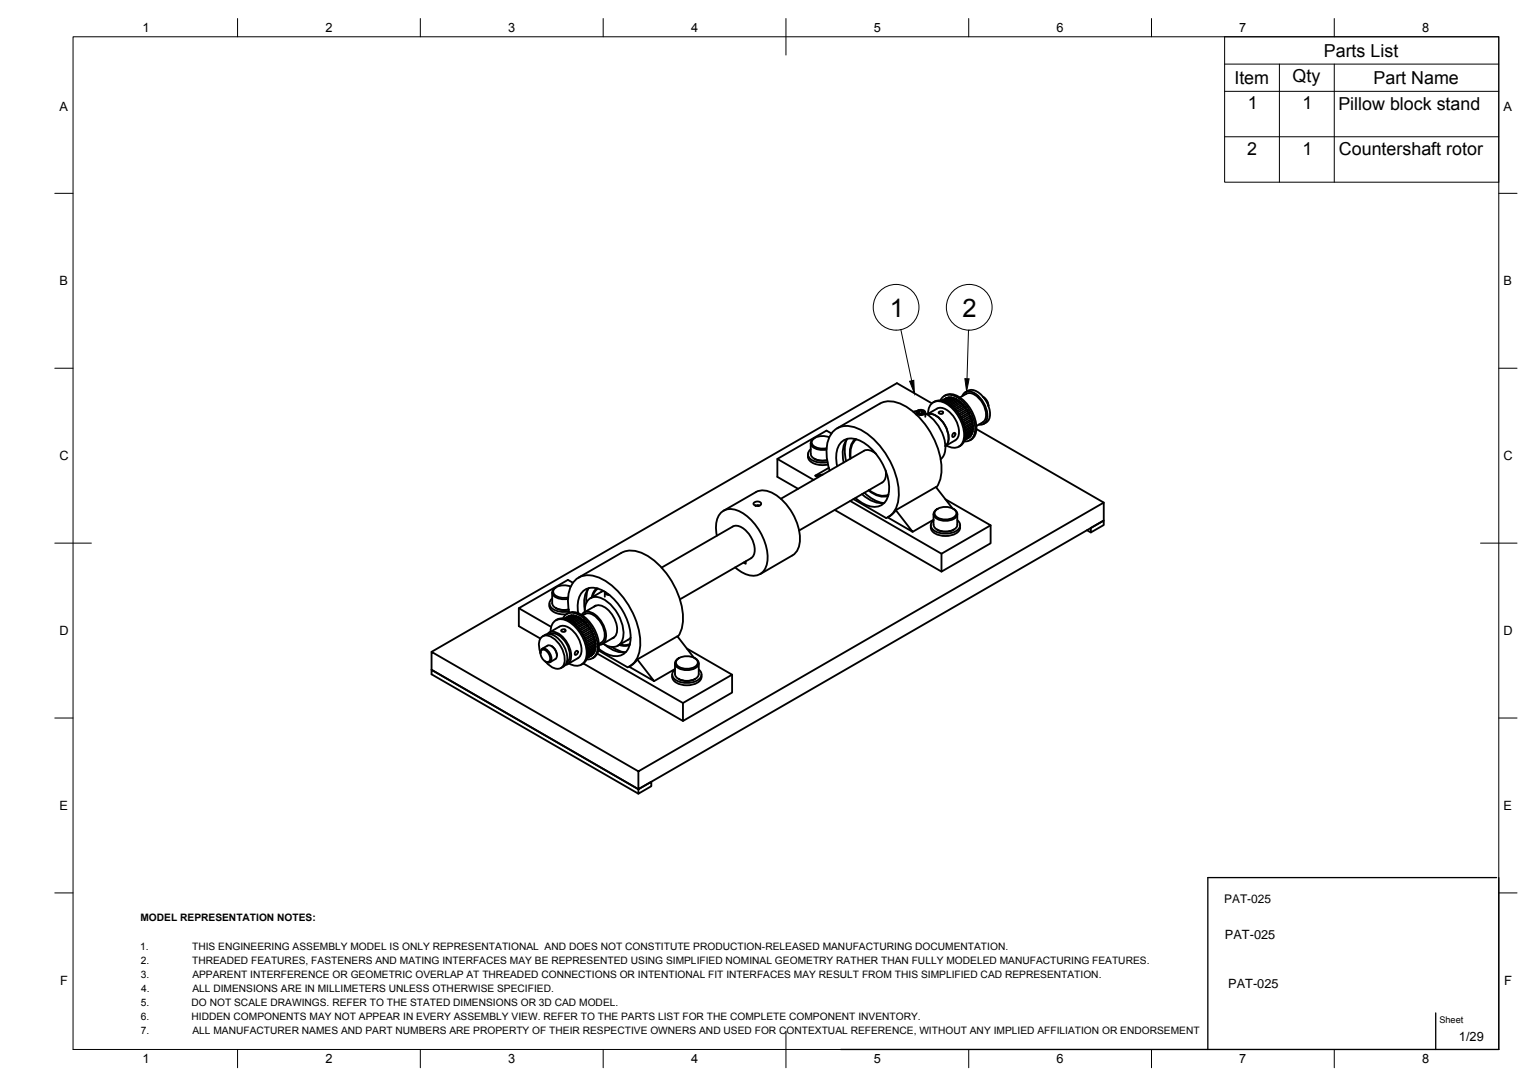
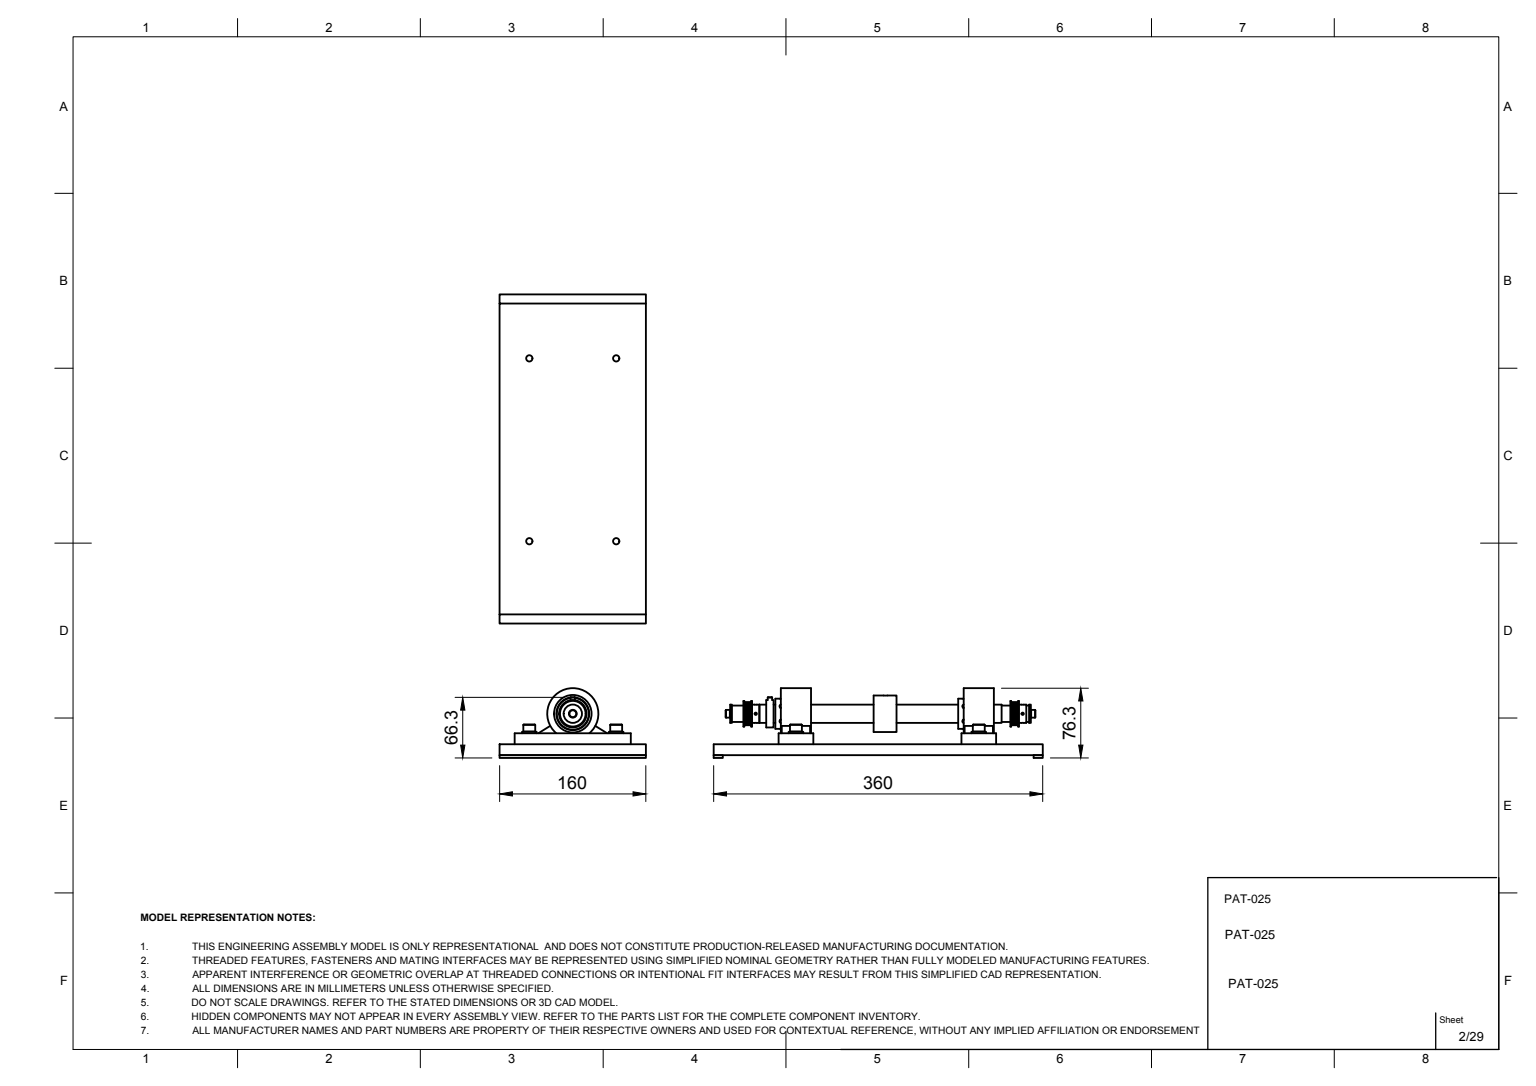
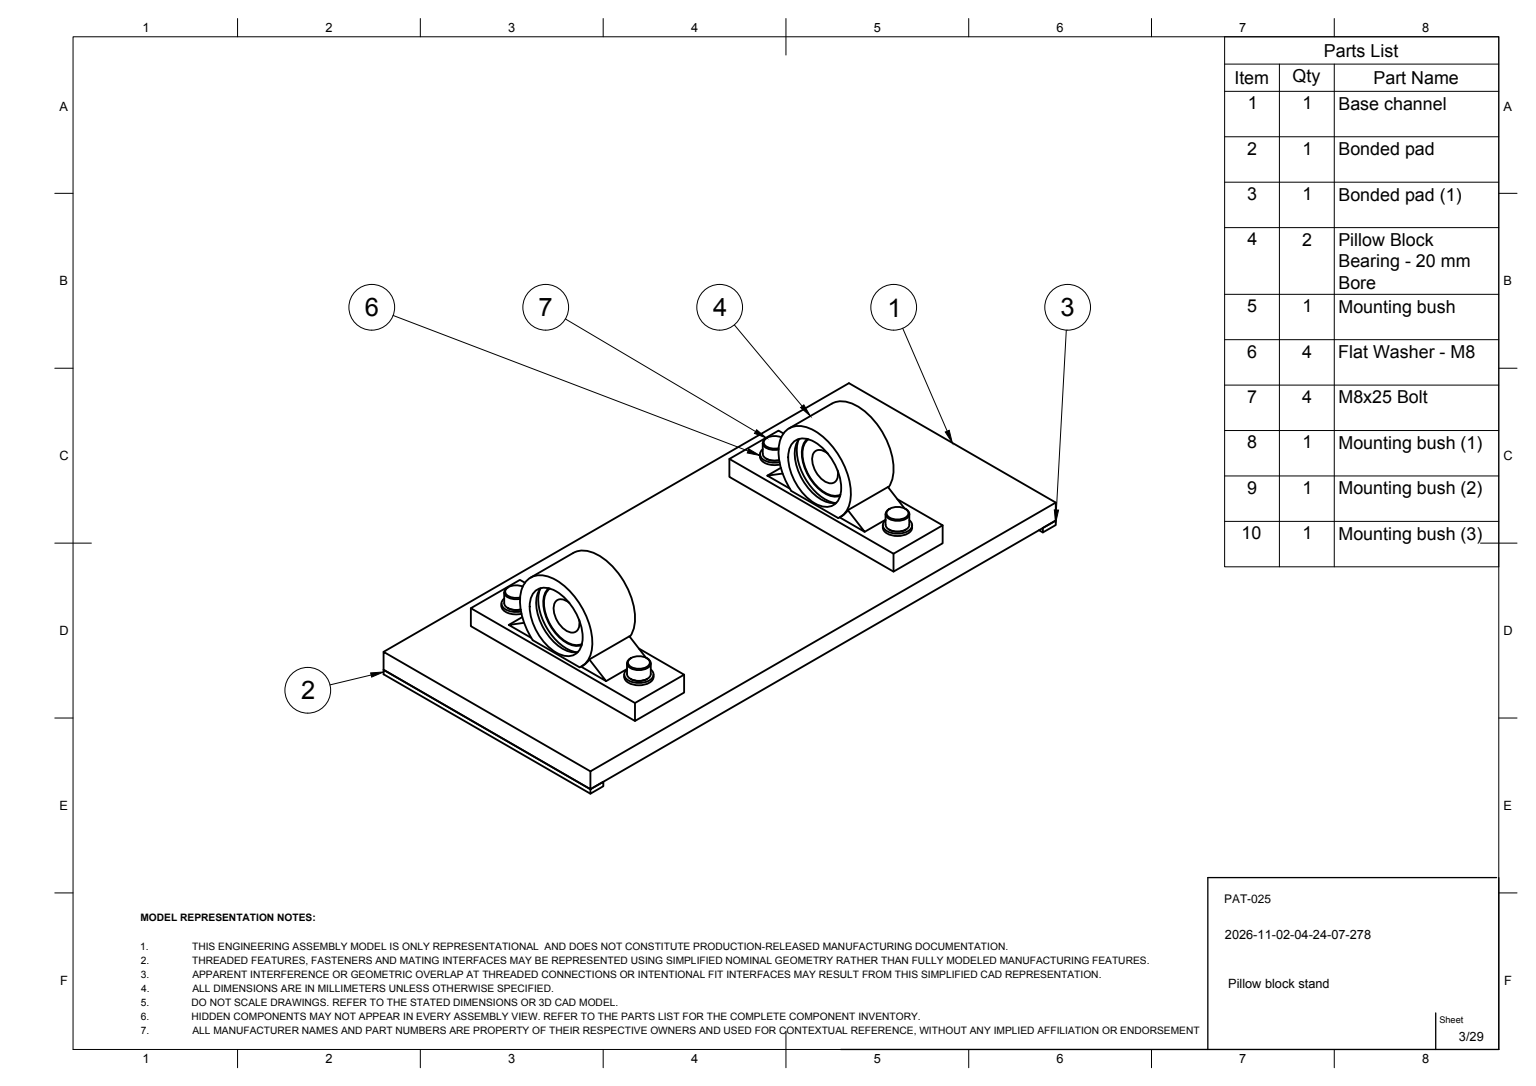
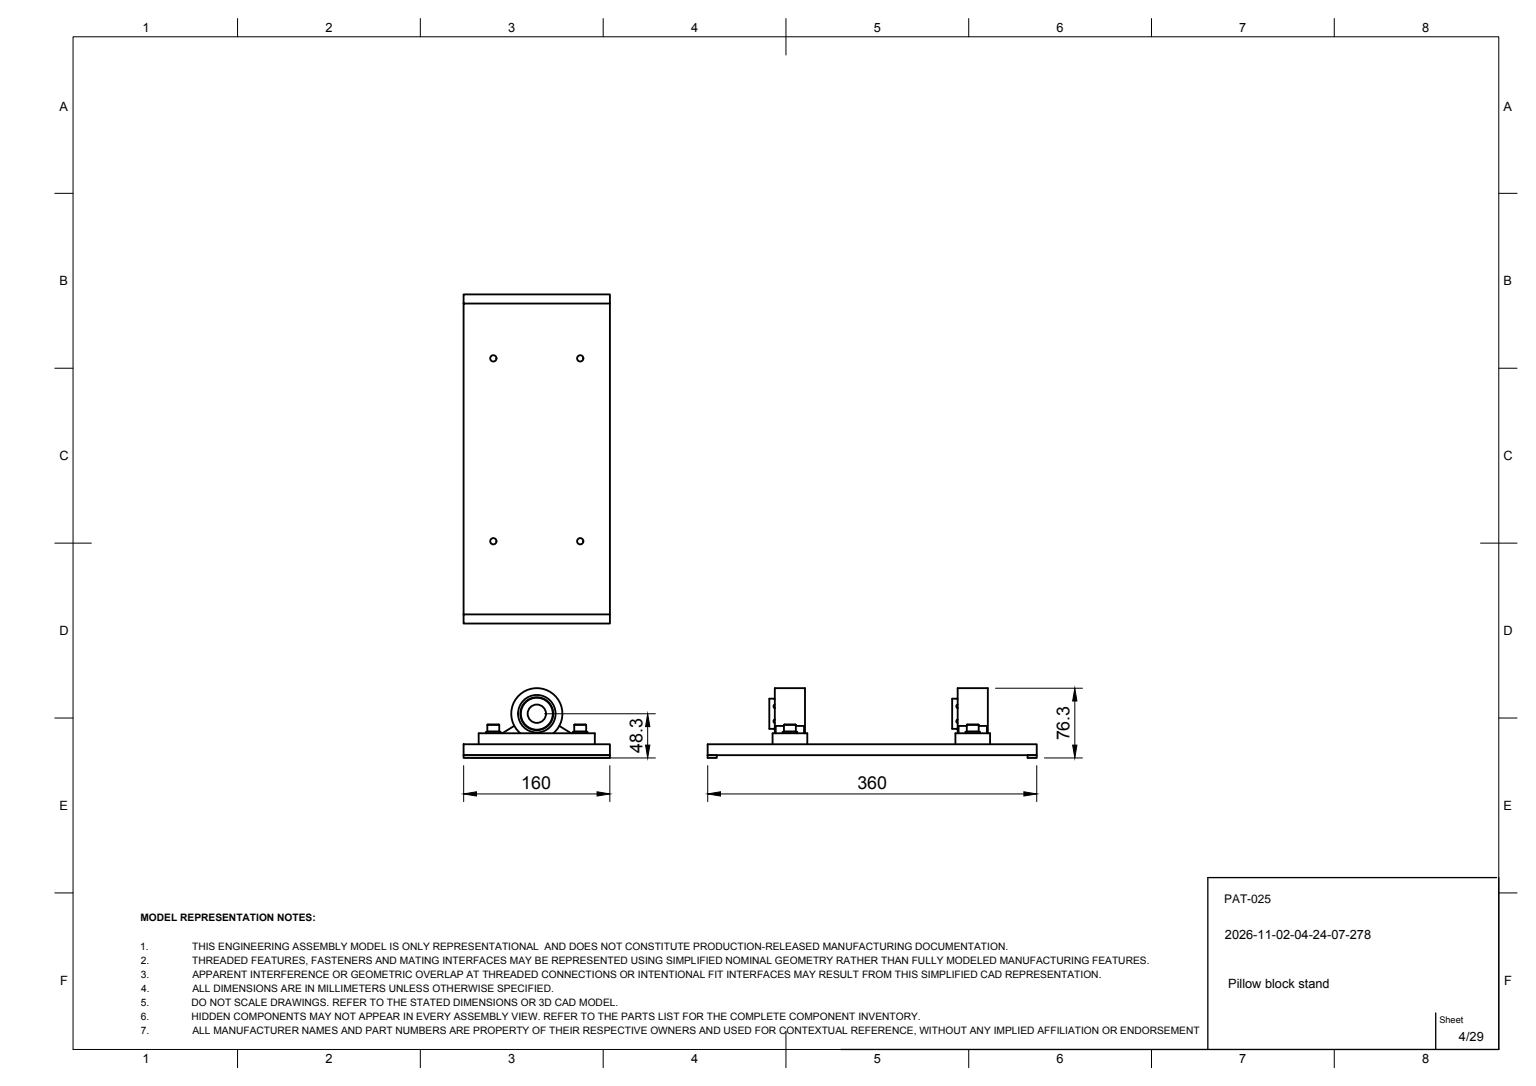
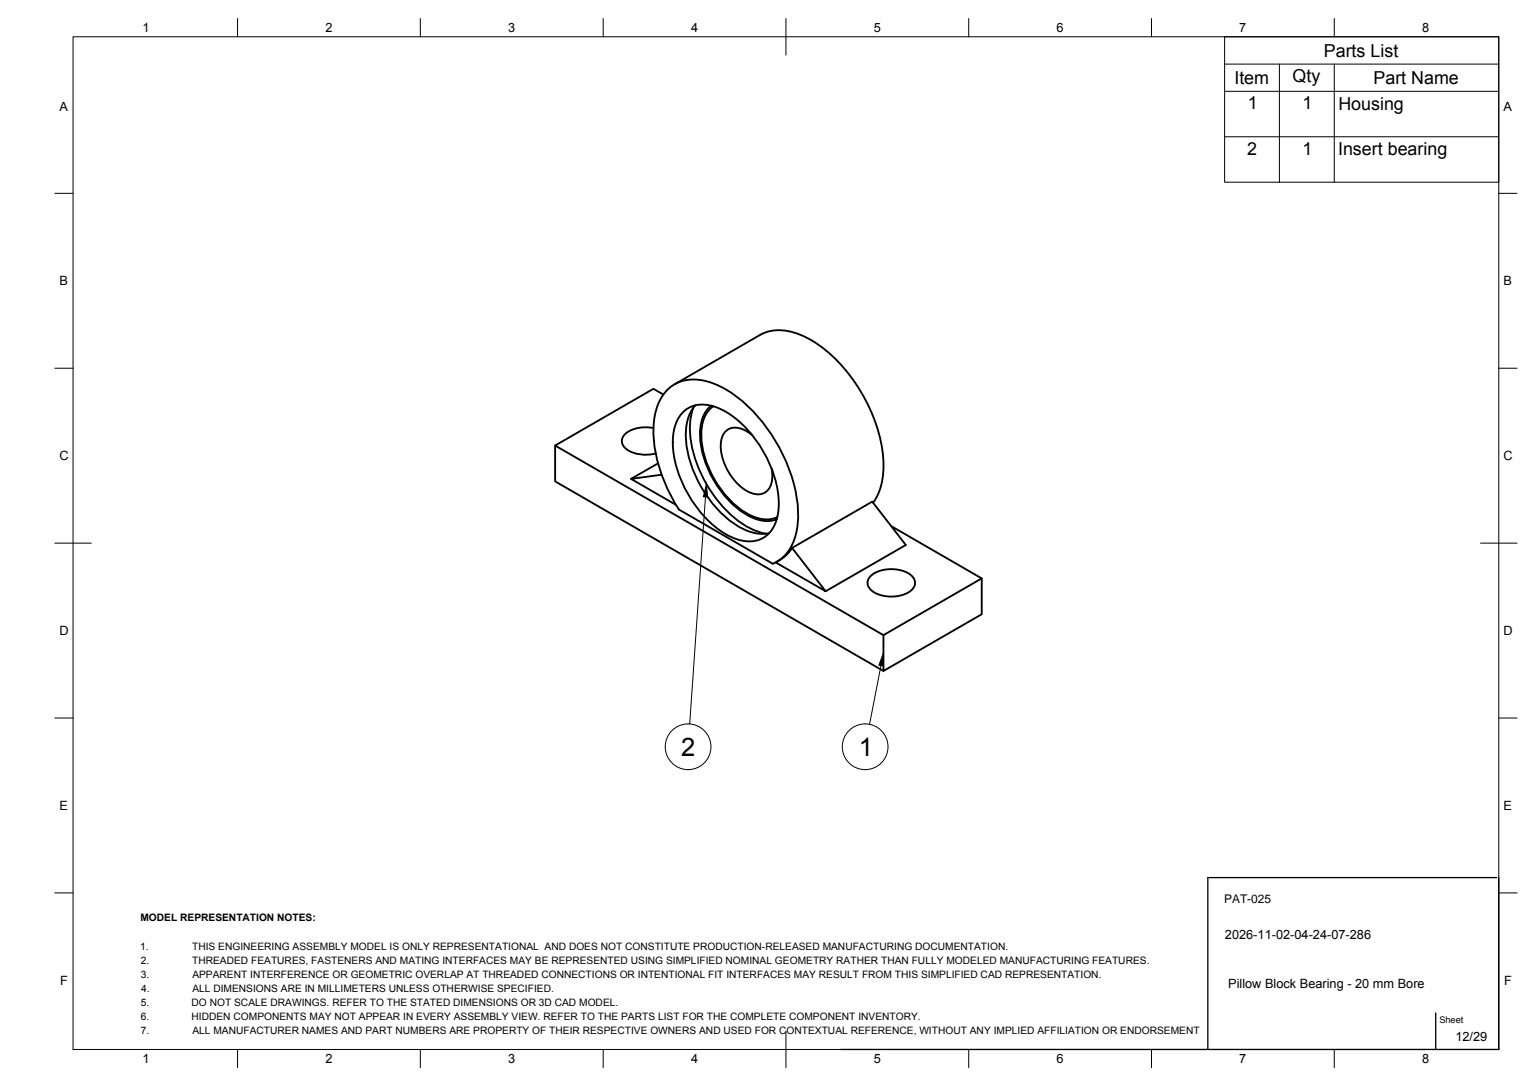
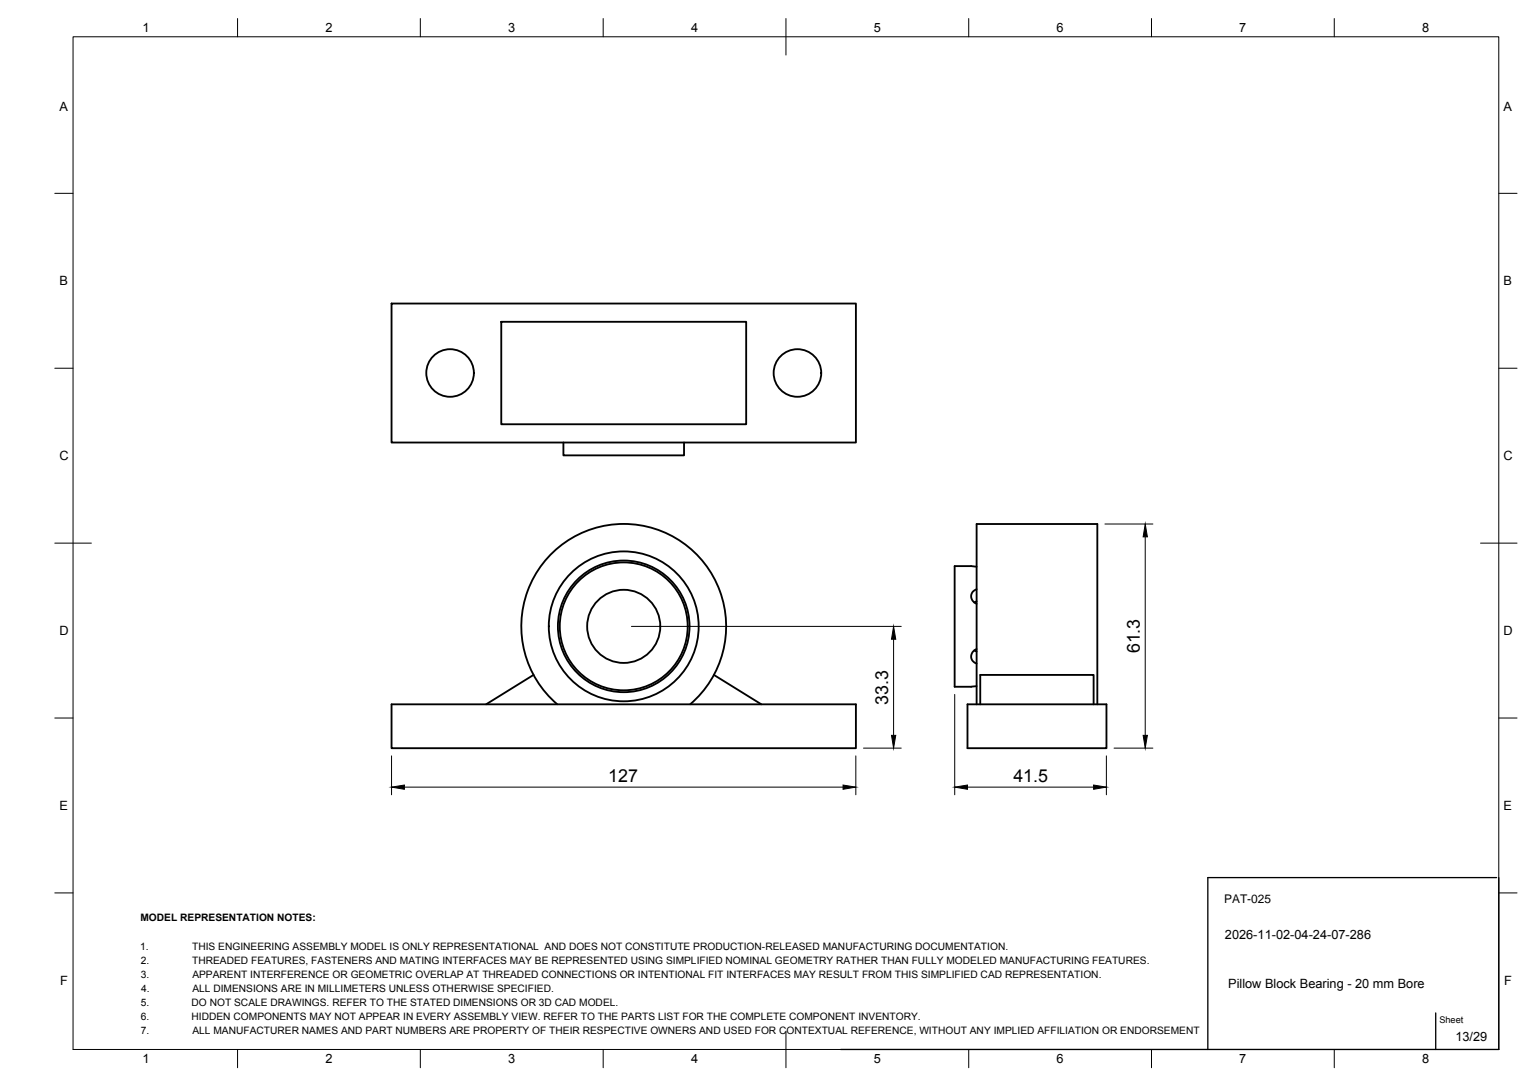
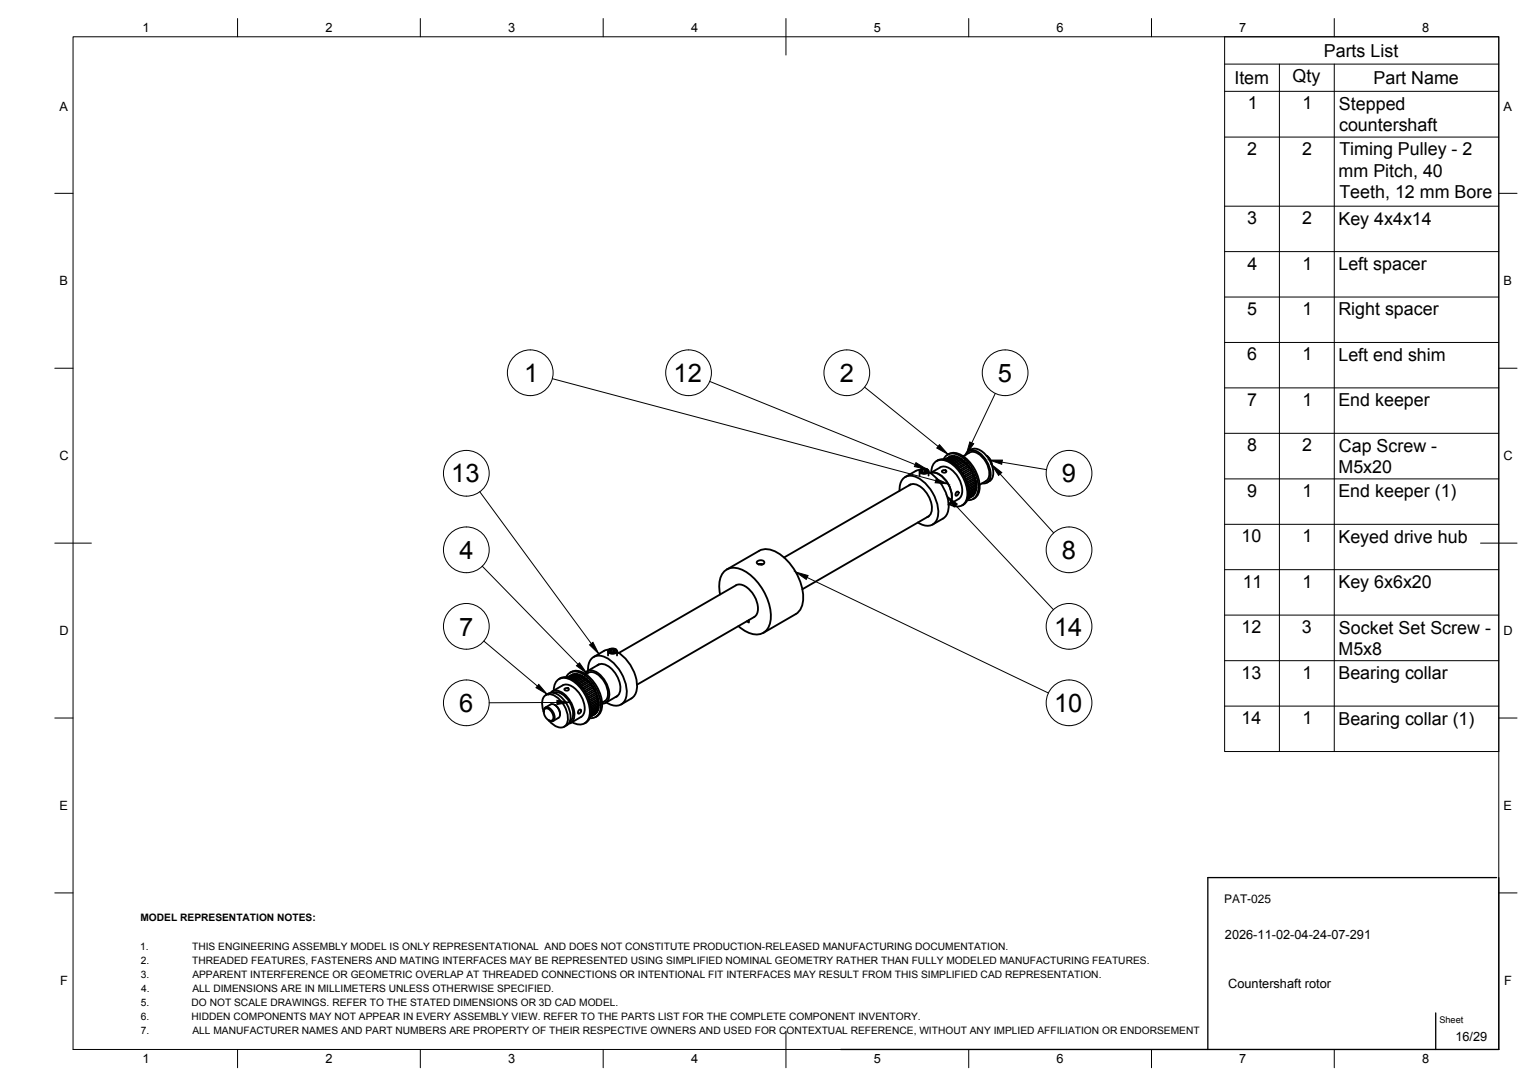
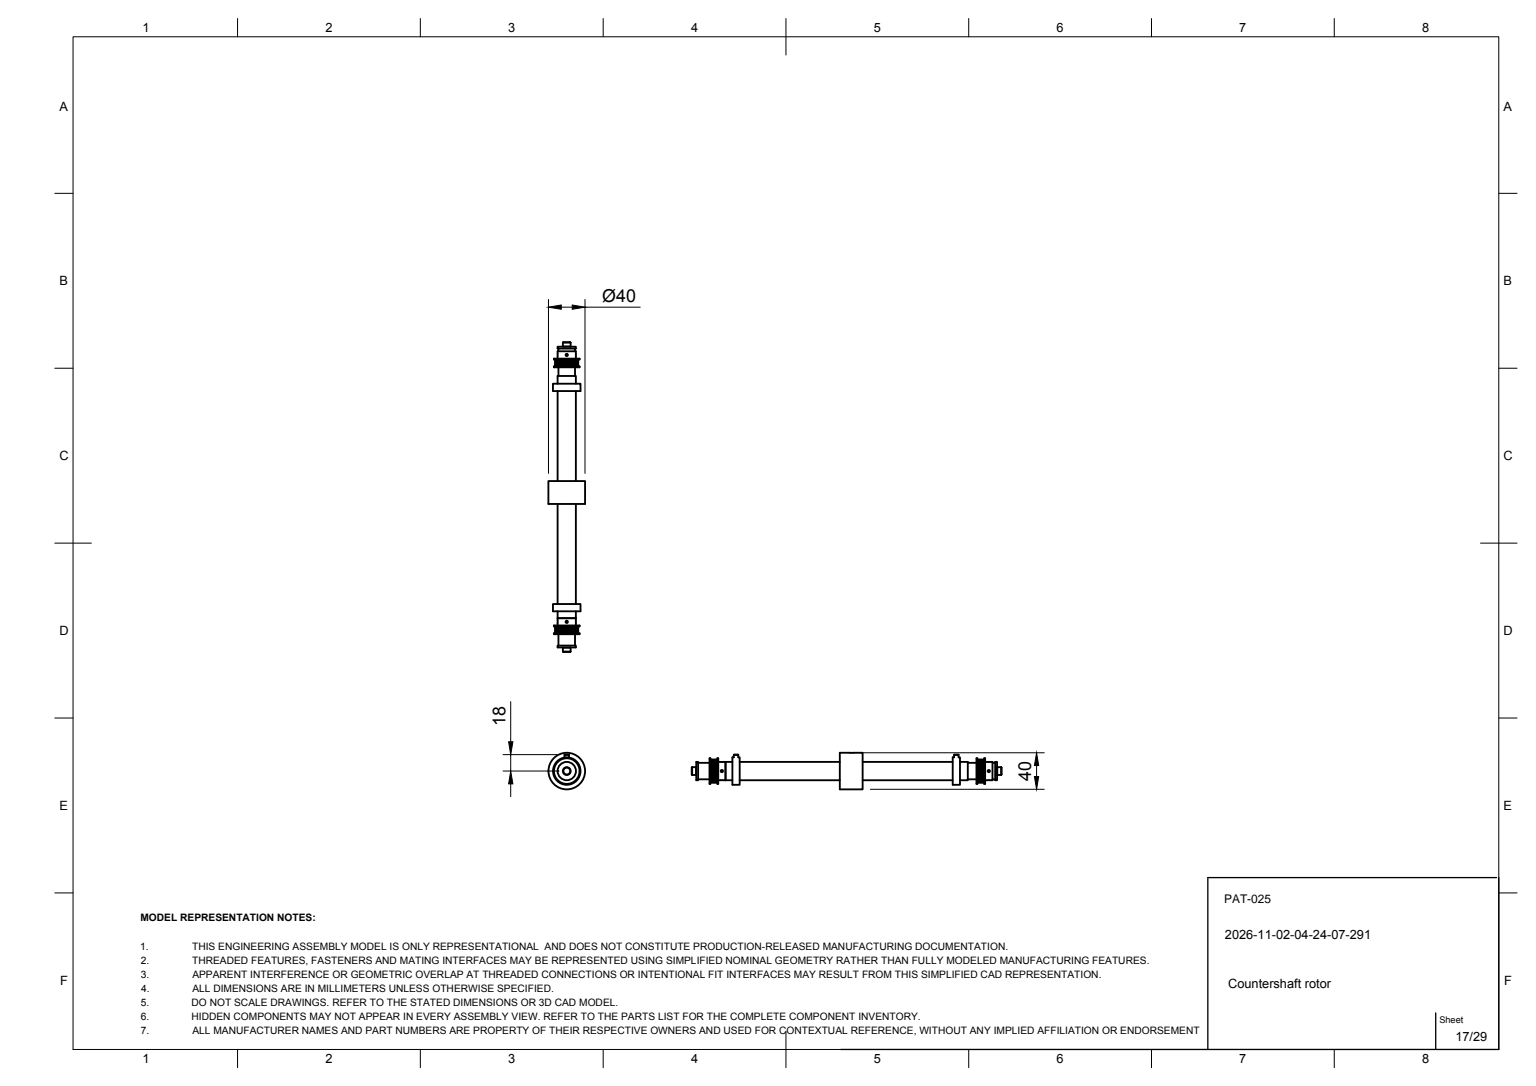
ISO-10303-21;
HEADER;
/* Generated by software containing ST-Developer
 * from STEP Tools, Inc. (www.steptools.com) 
 */

FILE_DESCRIPTION(
/* description */ ('Counter shaft with two pulleys and keyed hub'),
/* implementation_level */ '2;1');

FILE_NAME(
/* name */ 'PAT-025',
/* time_stamp */ '2026-10-27T10:46:10-07:00',
/* author */ (''),
/* organization */ (''),
/* preprocessor_version */ 'ST-DEVELOPER v20.2',
/* originating_system */ 'Autodesk Translation Framework v15.17.0.0',
/* authorisation */ '');

FILE_SCHEMA (('AUTOMOTIVE_DESIGN { 1 0 10303 214 3 1 1 }'));
ENDSEC;

DATA;
#10=MECHANICAL_DESIGN_GEOMETRIC_PRESENTATION_REPRESENTATION('',(#290,#291,
#292,#293,#294,#295,#296,#297,#298,#299,#300,#301,#302,#303,#304,#305,#306,
#307,#308,#309,#310,#311,#312,#313,#314,#315),#10821);
#11=CONICAL_SURFACE('',#6042,0.625,0.785398163397448);
#12=CONICAL_SURFACE('',#6046,0.635,0.785398163397449);
#13=CONICAL_SURFACE('',#6050,0.41,0.463647609000806);
#14=CONICAL_SURFACE('',#6487,0.4,0.785398163397448);
#15=CONICAL_SURFACE('',#6491,0.41,0.785398163397448);
#16=CONICAL_SURFACE('',#6495,0.26,0.463647609000806);
#17=CONICAL_SURFACE('',#6499,0.225,0.785398163397448);
#18=CONICAL_SURFACE('',#6531,0.235,0.785398163397448);
#19=CONICAL_SURFACE('',#6535,0.2125,0.785398163397448);
#20=ORIENTED_CLOSED_SHELL('',*,#5584,.F.);
#21=ORIENTED_CLOSED_SHELL('',*,#5598,.F.);
#22=BREP_WITH_VOIDS('Body1',#5585,(#20));
#23=BREP_WITH_VOIDS('Body1',#5597,(#21));
#24=ITEM_DEFINED_TRANSFORMATION($,$,#5949,#6018);
#25=ITEM_DEFINED_TRANSFORMATION($,$,#5990,#6019);
#26=ITEM_DEFINED_TRANSFORMATION($,$,#5879,#6053);
#27=ITEM_DEFINED_TRANSFORMATION($,$,#5898,#6054);
#28=ITEM_DEFINED_TRANSFORMATION($,$,#5905,#6055);
#29=ITEM_DEFINED_TRANSFORMATION($,$,#5912,#6056);
#30=ITEM_DEFINED_TRANSFORMATION($,$,#5921,#6057);
#31=ITEM_DEFINED_TRANSFORMATION($,$,#5930,#6058);
#32=ITEM_DEFINED_TRANSFORMATION($,$,#5939,#6059);
#33=ITEM_DEFINED_TRANSFORMATION($,$,#5948,#6060);
#34=ITEM_DEFINED_TRANSFORMATION($,$,#6020,#6061);
#35=ITEM_DEFINED_TRANSFORMATION($,$,#6029,#6062);
#36=ITEM_DEFINED_TRANSFORMATION($,$,#6020,#6063);
#37=ITEM_DEFINED_TRANSFORMATION($,$,#6029,#6064);
#38=ITEM_DEFINED_TRANSFORMATION($,$,#5948,#6065);
#39=ITEM_DEFINED_TRANSFORMATION($,$,#6020,#6066);
#40=ITEM_DEFINED_TRANSFORMATION($,$,#6029,#6067);
#41=ITEM_DEFINED_TRANSFORMATION($,$,#6020,#6068);
#42=ITEM_DEFINED_TRANSFORMATION($,$,#6029,#6069);
#43=ITEM_DEFINED_TRANSFORMATION($,$,#6071,#6538);
#44=ITEM_DEFINED_TRANSFORMATION($,$,#6114,#6539);
#45=ITEM_DEFINED_TRANSFORMATION($,$,#6123,#6540);
#46=ITEM_DEFINED_TRANSFORMATION($,$,#6132,#6541);
#47=ITEM_DEFINED_TRANSFORMATION($,$,#6141,#6542);
#48=ITEM_DEFINED_TRANSFORMATION($,$,#6150,#6543);
#49=ITEM_DEFINED_TRANSFORMATION($,$,#6159,#6544);
#50=ITEM_DEFINED_TRANSFORMATION($,$,#6177,#6545);
#51=ITEM_DEFINED_TRANSFORMATION($,$,#6192,#6546);
#52=ITEM_DEFINED_TRANSFORMATION($,$,#6207,#6547);
#53=ITEM_DEFINED_TRANSFORMATION($,$,#6473,#6548);
#54=ITEM_DEFINED_TRANSFORMATION($,$,#6207,#6549);
#55=ITEM_DEFINED_TRANSFORMATION($,$,#6473,#6550);
#56=ITEM_DEFINED_TRANSFORMATION($,$,#6484,#6551);
#57=ITEM_DEFINED_TRANSFORMATION($,$,#6484,#6552);
#58=ITEM_DEFINED_TRANSFORMATION($,$,#6510,#6553);
#59=ITEM_DEFINED_TRANSFORMATION($,$,#6521,#6554);
#60=ITEM_DEFINED_TRANSFORMATION($,$,#6521,#6555);
#61=ITEM_DEFINED_TRANSFORMATION($,$,#6521,#6556);
#62=ITEM_DEFINED_TRANSFORMATION($,$,#5878,#6557);
#63=ITEM_DEFINED_TRANSFORMATION($,$,#6070,#6558);
#64=(
REPRESENTATION_RELATIONSHIP($,$,#10934,#10933)
REPRESENTATION_RELATIONSHIP_WITH_TRANSFORMATION(#24)
SHAPE_REPRESENTATION_RELATIONSHIP()
);
#65=(
REPRESENTATION_RELATIONSHIP($,$,#10935,#10933)
REPRESENTATION_RELATIONSHIP_WITH_TRANSFORMATION(#25)
SHAPE_REPRESENTATION_RELATIONSHIP()
);
#66=(
REPRESENTATION_RELATIONSHIP($,$,#10926,#10925)
REPRESENTATION_RELATIONSHIP_WITH_TRANSFORMATION(#26)
SHAPE_REPRESENTATION_RELATIONSHIP()
);
#67=(
REPRESENTATION_RELATIONSHIP($,$,#10927,#10925)
REPRESENTATION_RELATIONSHIP_WITH_TRANSFORMATION(#27)
SHAPE_REPRESENTATION_RELATIONSHIP()
);
#68=(
REPRESENTATION_RELATIONSHIP($,$,#10928,#10925)
REPRESENTATION_RELATIONSHIP_WITH_TRANSFORMATION(#28)
SHAPE_REPRESENTATION_RELATIONSHIP()
);
#69=(
REPRESENTATION_RELATIONSHIP($,$,#10929,#10925)
REPRESENTATION_RELATIONSHIP_WITH_TRANSFORMATION(#29)
SHAPE_REPRESENTATION_RELATIONSHIP()
);
#70=(
REPRESENTATION_RELATIONSHIP($,$,#10930,#10925)
REPRESENTATION_RELATIONSHIP_WITH_TRANSFORMATION(#30)
SHAPE_REPRESENTATION_RELATIONSHIP()
);
#71=(
REPRESENTATION_RELATIONSHIP($,$,#10931,#10925)
REPRESENTATION_RELATIONSHIP_WITH_TRANSFORMATION(#31)
SHAPE_REPRESENTATION_RELATIONSHIP()
);
#72=(
REPRESENTATION_RELATIONSHIP($,$,#10932,#10925)
REPRESENTATION_RELATIONSHIP_WITH_TRANSFORMATION(#32)
SHAPE_REPRESENTATION_RELATIONSHIP()
);
#73=(
REPRESENTATION_RELATIONSHIP($,$,#10933,#10925)
REPRESENTATION_RELATIONSHIP_WITH_TRANSFORMATION(#33)
SHAPE_REPRESENTATION_RELATIONSHIP()
);
#74=(
REPRESENTATION_RELATIONSHIP($,$,#10936,#10925)
REPRESENTATION_RELATIONSHIP_WITH_TRANSFORMATION(#34)
SHAPE_REPRESENTATION_RELATIONSHIP()
);
#75=(
REPRESENTATION_RELATIONSHIP($,$,#10937,#10925)
REPRESENTATION_RELATIONSHIP_WITH_TRANSFORMATION(#35)
SHAPE_REPRESENTATION_RELATIONSHIP()
);
#76=(
REPRESENTATION_RELATIONSHIP($,$,#10936,#10925)
REPRESENTATION_RELATIONSHIP_WITH_TRANSFORMATION(#36)
SHAPE_REPRESENTATION_RELATIONSHIP()
);
#77=(
REPRESENTATION_RELATIONSHIP($,$,#10937,#10925)
REPRESENTATION_RELATIONSHIP_WITH_TRANSFORMATION(#37)
SHAPE_REPRESENTATION_RELATIONSHIP()
);
#78=(
REPRESENTATION_RELATIONSHIP($,$,#10933,#10925)
REPRESENTATION_RELATIONSHIP_WITH_TRANSFORMATION(#38)
SHAPE_REPRESENTATION_RELATIONSHIP()
);
#79=(
REPRESENTATION_RELATIONSHIP($,$,#10936,#10925)
REPRESENTATION_RELATIONSHIP_WITH_TRANSFORMATION(#39)
SHAPE_REPRESENTATION_RELATIONSHIP()
);
#80=(
REPRESENTATION_RELATIONSHIP($,$,#10937,#10925)
REPRESENTATION_RELATIONSHIP_WITH_TRANSFORMATION(#40)
SHAPE_REPRESENTATION_RELATIONSHIP()
);
#81=(
REPRESENTATION_RELATIONSHIP($,$,#10936,#10925)
REPRESENTATION_RELATIONSHIP_WITH_TRANSFORMATION(#41)
SHAPE_REPRESENTATION_RELATIONSHIP()
);
#82=(
REPRESENTATION_RELATIONSHIP($,$,#10937,#10925)
REPRESENTATION_RELATIONSHIP_WITH_TRANSFORMATION(#42)
SHAPE_REPRESENTATION_RELATIONSHIP()
);
#83=(
REPRESENTATION_RELATIONSHIP($,$,#10939,#10938)
REPRESENTATION_RELATIONSHIP_WITH_TRANSFORMATION(#43)
SHAPE_REPRESENTATION_RELATIONSHIP()
);
#84=(
REPRESENTATION_RELATIONSHIP($,$,#10940,#10938)
REPRESENTATION_RELATIONSHIP_WITH_TRANSFORMATION(#44)
SHAPE_REPRESENTATION_RELATIONSHIP()
);
#85=(
REPRESENTATION_RELATIONSHIP($,$,#10941,#10938)
REPRESENTATION_RELATIONSHIP_WITH_TRANSFORMATION(#45)
SHAPE_REPRESENTATION_RELATIONSHIP()
);
#86=(
REPRESENTATION_RELATIONSHIP($,$,#10942,#10938)
REPRESENTATION_RELATIONSHIP_WITH_TRANSFORMATION(#46)
SHAPE_REPRESENTATION_RELATIONSHIP()
);
#87=(
REPRESENTATION_RELATIONSHIP($,$,#10943,#10938)
REPRESENTATION_RELATIONSHIP_WITH_TRANSFORMATION(#47)
SHAPE_REPRESENTATION_RELATIONSHIP()
);
#88=(
REPRESENTATION_RELATIONSHIP($,$,#10944,#10938)
REPRESENTATION_RELATIONSHIP_WITH_TRANSFORMATION(#48)
SHAPE_REPRESENTATION_RELATIONSHIP()
);
#89=(
REPRESENTATION_RELATIONSHIP($,$,#10945,#10938)
REPRESENTATION_RELATIONSHIP_WITH_TRANSFORMATION(#49)
SHAPE_REPRESENTATION_RELATIONSHIP()
);
#90=(
REPRESENTATION_RELATIONSHIP($,$,#10946,#10938)
REPRESENTATION_RELATIONSHIP_WITH_TRANSFORMATION(#50)
SHAPE_REPRESENTATION_RELATIONSHIP()
);
#91=(
REPRESENTATION_RELATIONSHIP($,$,#10947,#10938)
REPRESENTATION_RELATIONSHIP_WITH_TRANSFORMATION(#51)
SHAPE_REPRESENTATION_RELATIONSHIP()
);
#92=(
REPRESENTATION_RELATIONSHIP($,$,#10948,#10938)
REPRESENTATION_RELATIONSHIP_WITH_TRANSFORMATION(#52)
SHAPE_REPRESENTATION_RELATIONSHIP()
);
#93=(
REPRESENTATION_RELATIONSHIP($,$,#10949,#10938)
REPRESENTATION_RELATIONSHIP_WITH_TRANSFORMATION(#53)
SHAPE_REPRESENTATION_RELATIONSHIP()
);
#94=(
REPRESENTATION_RELATIONSHIP($,$,#10948,#10938)
REPRESENTATION_RELATIONSHIP_WITH_TRANSFORMATION(#54)
SHAPE_REPRESENTATION_RELATIONSHIP()
);
#95=(
REPRESENTATION_RELATIONSHIP($,$,#10949,#10938)
REPRESENTATION_RELATIONSHIP_WITH_TRANSFORMATION(#55)
SHAPE_REPRESENTATION_RELATIONSHIP()
);
#96=(
REPRESENTATION_RELATIONSHIP($,$,#10950,#10938)
REPRESENTATION_RELATIONSHIP_WITH_TRANSFORMATION(#56)
SHAPE_REPRESENTATION_RELATIONSHIP()
);
#97=(
REPRESENTATION_RELATIONSHIP($,$,#10950,#10938)
REPRESENTATION_RELATIONSHIP_WITH_TRANSFORMATION(#57)
SHAPE_REPRESENTATION_RELATIONSHIP()
);
#98=(
REPRESENTATION_RELATIONSHIP($,$,#10951,#10938)
REPRESENTATION_RELATIONSHIP_WITH_TRANSFORMATION(#58)
SHAPE_REPRESENTATION_RELATIONSHIP()
);
#99=(
REPRESENTATION_RELATIONSHIP($,$,#10952,#10938)
REPRESENTATION_RELATIONSHIP_WITH_TRANSFORMATION(#59)
SHAPE_REPRESENTATION_RELATIONSHIP()
);
#100=(
REPRESENTATION_RELATIONSHIP($,$,#10952,#10938)
REPRESENTATION_RELATIONSHIP_WITH_TRANSFORMATION(#60)
SHAPE_REPRESENTATION_RELATIONSHIP()
);
#101=(
REPRESENTATION_RELATIONSHIP($,$,#10952,#10938)
REPRESENTATION_RELATIONSHIP_WITH_TRANSFORMATION(#61)
SHAPE_REPRESENTATION_RELATIONSHIP()
);
#102=(
REPRESENTATION_RELATIONSHIP($,$,#10925,#10924)
REPRESENTATION_RELATIONSHIP_WITH_TRANSFORMATION(#62)
SHAPE_REPRESENTATION_RELATIONSHIP()
);
#103=(
REPRESENTATION_RELATIONSHIP($,$,#10938,#10924)
REPRESENTATION_RELATIONSHIP_WITH_TRANSFORMATION(#63)
SHAPE_REPRESENTATION_RELATIONSHIP()
);
#104=CONTEXT_DEPENDENT_SHAPE_REPRESENTATION(#64,#10867);
#105=CONTEXT_DEPENDENT_SHAPE_REPRESENTATION(#65,#10868);
#106=CONTEXT_DEPENDENT_SHAPE_REPRESENTATION(#66,#10871);
#107=CONTEXT_DEPENDENT_SHAPE_REPRESENTATION(#67,#10872);
#108=CONTEXT_DEPENDENT_SHAPE_REPRESENTATION(#68,#10873);
#109=CONTEXT_DEPENDENT_SHAPE_REPRESENTATION(#69,#10874);
#110=CONTEXT_DEPENDENT_SHAPE_REPRESENTATION(#70,#10875);
#111=CONTEXT_DEPENDENT_SHAPE_REPRESENTATION(#71,#10876);
#112=CONTEXT_DEPENDENT_SHAPE_REPRESENTATION(#72,#10877);
#113=CONTEXT_DEPENDENT_SHAPE_REPRESENTATION(#73,#10878);
#114=CONTEXT_DEPENDENT_SHAPE_REPRESENTATION(#74,#10879);
#115=CONTEXT_DEPENDENT_SHAPE_REPRESENTATION(#75,#10880);
#116=CONTEXT_DEPENDENT_SHAPE_REPRESENTATION(#76,#10881);
#117=CONTEXT_DEPENDENT_SHAPE_REPRESENTATION(#77,#10882);
#118=CONTEXT_DEPENDENT_SHAPE_REPRESENTATION(#78,#10883);
#119=CONTEXT_DEPENDENT_SHAPE_REPRESENTATION(#79,#10884);
#120=CONTEXT_DEPENDENT_SHAPE_REPRESENTATION(#80,#10885);
#121=CONTEXT_DEPENDENT_SHAPE_REPRESENTATION(#81,#10886);
#122=CONTEXT_DEPENDENT_SHAPE_REPRESENTATION(#82,#10887);
#123=CONTEXT_DEPENDENT_SHAPE_REPRESENTATION(#83,#10903);
#124=CONTEXT_DEPENDENT_SHAPE_REPRESENTATION(#84,#10904);
#125=CONTEXT_DEPENDENT_SHAPE_REPRESENTATION(#85,#10905);
#126=CONTEXT_DEPENDENT_SHAPE_REPRESENTATION(#86,#10906);
#127=CONTEXT_DEPENDENT_SHAPE_REPRESENTATION(#87,#10907);
#128=CONTEXT_DEPENDENT_SHAPE_REPRESENTATION(#88,#10908);
#129=CONTEXT_DEPENDENT_SHAPE_REPRESENTATION(#89,#10909);
#130=CONTEXT_DEPENDENT_SHAPE_REPRESENTATION(#90,#10910);
#131=CONTEXT_DEPENDENT_SHAPE_REPRESENTATION(#91,#10911);
#132=CONTEXT_DEPENDENT_SHAPE_REPRESENTATION(#92,#10912);
#133=CONTEXT_DEPENDENT_SHAPE_REPRESENTATION(#93,#10913);
#134=CONTEXT_DEPENDENT_SHAPE_REPRESENTATION(#94,#10914);
#135=CONTEXT_DEPENDENT_SHAPE_REPRESENTATION(#95,#10915);
#136=CONTEXT_DEPENDENT_SHAPE_REPRESENTATION(#96,#10916);
#137=CONTEXT_DEPENDENT_SHAPE_REPRESENTATION(#97,#10917);
#138=CONTEXT_DEPENDENT_SHAPE_REPRESENTATION(#98,#10918);
#139=CONTEXT_DEPENDENT_SHAPE_REPRESENTATION(#99,#10919);
#140=CONTEXT_DEPENDENT_SHAPE_REPRESENTATION(#100,#10920);
#141=CONTEXT_DEPENDENT_SHAPE_REPRESENTATION(#101,#10921);
#142=CONTEXT_DEPENDENT_SHAPE_REPRESENTATION(#102,#10922);
#143=CONTEXT_DEPENDENT_SHAPE_REPRESENTATION(#103,#10923);
#144=NEXT_ASSEMBLY_USAGE_OCCURRENCE('Housing:1','Housing:1','Housing:1',
#10963,#10964,'Housing:1');
#145=NEXT_ASSEMBLY_USAGE_OCCURRENCE('Insert bearing:1',
'Insert bearing:1','Insert bearing:1',#10963,#10965,'Insert bearing:1');
#146=NEXT_ASSEMBLY_USAGE_OCCURRENCE('Base channel:1','Base channel:1',
'Base channel:1',#10955,#10956,'Base channel:1');
#147=NEXT_ASSEMBLY_USAGE_OCCURRENCE('Bonded pad:1','Bonded pad:1',
'Bonded pad:1',#10955,#10957,'Bonded pad:1');
#148=NEXT_ASSEMBLY_USAGE_OCCURRENCE('Bonded pad (1):1',
'Bonded pad (1):1','Bonded pad (1):1',#10955,#10958,'Bonded pad (1):1');
#149=NEXT_ASSEMBLY_USAGE_OCCURRENCE('Mounting bush:1','Mounting bush:1',
'Mounting bush:1',#10955,#10959,'Mounting bush:1');
#150=NEXT_ASSEMBLY_USAGE_OCCURRENCE('Mounting bush (1):1',
'Mounting bush (1):1','Mounting bush (1):1',#10955,#10960,
'Mounting bush (1):1');
#151=NEXT_ASSEMBLY_USAGE_OCCURRENCE('Mounting bush (2):1',
'Mounting bush (2):1','Mounting bush (2):1',#10955,#10961,
'Mounting bush (2):1');
#152=NEXT_ASSEMBLY_USAGE_OCCURRENCE('Mounting bush (3):1',
'Mounting bush (3):1','Mounting bush (3):1',#10955,#10962,
'Mounting bush (3):1');
#153=NEXT_ASSEMBLY_USAGE_OCCURRENCE(
'Pillow Block Bearing - 20 mm Bore:2',
'Pillow Block Bearing - 20 mm Bore:2',
'Pillow Block Bearing - 20 mm Bore:2',#10955,#10963,
'Pillow Block Bearing - 20 mm Bore:2');
#154=NEXT_ASSEMBLY_USAGE_OCCURRENCE('Flat Washer - M8:2',
'Flat Washer - M8:2','Flat Washer - M8:2',#10955,#10966,
'Flat Washer - M8:2');
#155=NEXT_ASSEMBLY_USAGE_OCCURRENCE('M8x25 Bolt:2','M8x25 Bolt:2',
'M8x25 Bolt:2',#10955,#10967,'M8x25 Bolt:2');
#156=NEXT_ASSEMBLY_USAGE_OCCURRENCE('Flat Washer - M8:3',
'Flat Washer - M8:3','Flat Washer - M8:3',#10955,#10966,
'Flat Washer - M8:3');
#157=NEXT_ASSEMBLY_USAGE_OCCURRENCE('M8x25 Bolt:3','M8x25 Bolt:3',
'M8x25 Bolt:3',#10955,#10967,'M8x25 Bolt:3');
#158=NEXT_ASSEMBLY_USAGE_OCCURRENCE(
'Pillow Block Bearing - 20 mm Bore:3',
'Pillow Block Bearing - 20 mm Bore:3',
'Pillow Block Bearing - 20 mm Bore:3',#10955,#10963,
'Pillow Block Bearing - 20 mm Bore:3');
#159=NEXT_ASSEMBLY_USAGE_OCCURRENCE('Flat Washer - M8:4',
'Flat Washer - M8:4','Flat Washer - M8:4',#10955,#10966,
'Flat Washer - M8:4');
#160=NEXT_ASSEMBLY_USAGE_OCCURRENCE('M8x25 Bolt:4','M8x25 Bolt:4',
'M8x25 Bolt:4',#10955,#10967,'M8x25 Bolt:4');
#161=NEXT_ASSEMBLY_USAGE_OCCURRENCE('Flat Washer - M8:5',
'Flat Washer - M8:5','Flat Washer - M8:5',#10955,#10966,
'Flat Washer - M8:5');
#162=NEXT_ASSEMBLY_USAGE_OCCURRENCE('M8x25 Bolt:5','M8x25 Bolt:5',
'M8x25 Bolt:5',#10955,#10967,'M8x25 Bolt:5');
#163=NEXT_ASSEMBLY_USAGE_OCCURRENCE('Stepped countershaft:1',
'Stepped countershaft:1','Stepped countershaft:1',#10968,#10969,
'Stepped countershaft:1');
#164=NEXT_ASSEMBLY_USAGE_OCCURRENCE('Left spacer:1','Left spacer:1',
'Left spacer:1',#10968,#10970,'Left spacer:1');
#165=NEXT_ASSEMBLY_USAGE_OCCURRENCE('Right spacer:1','Right spacer:1',
'Right spacer:1',#10968,#10971,'Right spacer:1');
#166=NEXT_ASSEMBLY_USAGE_OCCURRENCE('Left end shim:1','Left end shim:1',
'Left end shim:1',#10968,#10972,'Left end shim:1');
#167=NEXT_ASSEMBLY_USAGE_OCCURRENCE('End keeper:1','End keeper:1',
'End keeper:1',#10968,#10973,'End keeper:1');
#168=NEXT_ASSEMBLY_USAGE_OCCURRENCE('End keeper (1):1',
'End keeper (1):1','End keeper (1):1',#10968,#10974,'End keeper (1):1');
#169=NEXT_ASSEMBLY_USAGE_OCCURRENCE('Keyed drive hub:1',
'Keyed drive hub:1','Keyed drive hub:1',#10968,#10975,
'Keyed drive hub:1');
#170=NEXT_ASSEMBLY_USAGE_OCCURRENCE('Bearing collar:1',
'Bearing collar:1','Bearing collar:1',#10968,#10976,'Bearing collar:1');
#171=NEXT_ASSEMBLY_USAGE_OCCURRENCE('Bearing collar (1):1',
'Bearing collar (1):1','Bearing collar (1):1',#10968,#10977,
'Bearing collar (1):1');
#172=NEXT_ASSEMBLY_USAGE_OCCURRENCE(
'Timing Pulley - 2 mm Pitch, 40 Teeth, 12 mm Bore:2',
'Timing Pulley - 2 mm Pitch, 40 Teeth, 12 mm Bore:2',
'Timing Pulley - 2 mm Pitch, 40 Teeth, 12 mm Bore:2',#10968,#10978,
'Timing Pulley - 2 mm Pitch, 40 Teeth, 12 mm Bore:2');
#173=NEXT_ASSEMBLY_USAGE_OCCURRENCE('Key 4x4x14:2','Key 4x4x14:2',
'Key 4x4x14:2',#10968,#10979,'Key 4x4x14:2');
#174=NEXT_ASSEMBLY_USAGE_OCCURRENCE(
'Timing Pulley - 2 mm Pitch, 40 Teeth, 12 mm Bore:3',
'Timing Pulley - 2 mm Pitch, 40 Teeth, 12 mm Bore:3',
'Timing Pulley - 2 mm Pitch, 40 Teeth, 12 mm Bore:3',#10968,#10978,
'Timing Pulley - 2 mm Pitch, 40 Teeth, 12 mm Bore:3');
#175=NEXT_ASSEMBLY_USAGE_OCCURRENCE('Key 4x4x14:3','Key 4x4x14:3',
'Key 4x4x14:3',#10968,#10979,'Key 4x4x14:3');
#176=NEXT_ASSEMBLY_USAGE_OCCURRENCE('Cap Screw - M5x20:2',
'Cap Screw - M5x20:2','Cap Screw - M5x20:2',#10968,#10980,
'Cap Screw - M5x20:2');
#177=NEXT_ASSEMBLY_USAGE_OCCURRENCE('Cap Screw - M5x20:3',
'Cap Screw - M5x20:3','Cap Screw - M5x20:3',#10968,#10980,
'Cap Screw - M5x20:3');
#178=NEXT_ASSEMBLY_USAGE_OCCURRENCE('Key 6x6x20:2','Key 6x6x20:2',
'Key 6x6x20:2',#10968,#10981,'Key 6x6x20:2');
#179=NEXT_ASSEMBLY_USAGE_OCCURRENCE('Socket Set Screw - M5x8:2',
'Socket Set Screw - M5x8:2','Socket Set Screw - M5x8:2',#10968,#10982,
'Socket Set Screw - M5x8:2');
#180=NEXT_ASSEMBLY_USAGE_OCCURRENCE('Socket Set Screw - M5x8:3',
'Socket Set Screw - M5x8:3','Socket Set Screw - M5x8:3',#10968,#10982,
'Socket Set Screw - M5x8:3');
#181=NEXT_ASSEMBLY_USAGE_OCCURRENCE('Socket Set Screw - M5x8:4',
'Socket Set Screw - M5x8:4','Socket Set Screw - M5x8:4',#10968,#10982,
'Socket Set Screw - M5x8:4');
#182=NEXT_ASSEMBLY_USAGE_OCCURRENCE('Pillow block stand:1',
'Pillow block stand:1','Pillow block stand:1',#10954,#10955,
'Pillow block stand:1');
#183=NEXT_ASSEMBLY_USAGE_OCCURRENCE('Countershaft rotor:1',
'Countershaft rotor:1','Countershaft rotor:1',#10954,#10968,
'Countershaft rotor:1');
#184=B_SPLINE_CURVE_WITH_KNOTS('',3,(#8629,#8630,#8631,#8632,#8633,#8634,
#8635,#8636,#8637,#8638),.UNSPECIFIED.,.F.,.F.,(4,2,2,2,4),(1.13193471301885,
1.22626174930539,1.32058878559194,1.41491753480854,1.50924628402513),
 .UNSPECIFIED.);
#185=B_SPLINE_CURVE_WITH_KNOTS('',3,(#8640,#8641,#8642,#8643,#8644,#8645,
#8646,#8647,#8648,#8649,#8650,#8651,#8652,#8653,#8654,#8655,#8656,#8657),
 .UNSPECIFIED.,.F.,.F.,(4,2,2,2,2,2,2,2,4),(0.377311571006283,0.471638607292829,
0.565965643579376,0.66029439279597,0.754623142012565,0.84895189122916,0.943280640445754,
1.0376076767323,1.13193471301885),.UNSPECIFIED.);
#186=B_SPLINE_CURVE_WITH_KNOTS('',3,(#8658,#8659,#8660,#8661,#8662,#8663,
#8664,#8665,#8666,#8667),.UNSPECIFIED.,.F.,.F.,(4,2,2,2,4),(1.50924628402513,
1.60357503324173,1.69790378245832,1.79223081874487,1.88655785503141),
 .UNSPECIFIED.);
#187=B_SPLINE_CURVE_WITH_KNOTS('',3,(#8670,#8671,#8672,#8673,#8674,#8675,
#8676,#8677,#8678,#8679,#8680,#8681,#8682,#8683,#8684,#8685,#8686,#8687,
#8688,#8689,#8690,#8691,#8692,#8693,#8694,#8695,#8696,#8697,#8698,#8699,
#8700,#8701,#8702,#8703),.UNSPECIFIED.,.T.,.F.,(4,2,2,2,2,2,2,2,2,2,2,2,
2,2,2,2,4),(0.,0.0946120580087934,0.189224116017587,0.283822945575014,0.378421775132442,
0.47302060468987,0.567619434247297,0.662231492256091,0.756843550264884,
0.851455608273677,0.94606766628247,1.0406664958399,1.13526532539733,1.22986415495475,
1.32446298451218,1.41907504252097,1.51368710052977),.UNSPECIFIED.);
#188=B_SPLINE_CURVE_WITH_KNOTS('',3,(#8706,#8707,#8708,#8709,#8710,#8711,
#8712,#8713,#8714,#8715,#8716,#8717,#8718,#8719,#8720,#8721,#8722,#8723,
#8724,#8725,#8726,#8727,#8728,#8729,#8730,#8731,#8732,#8733,#8734,#8735,
#8736,#8737,#8738,#8739),.UNSPECIFIED.,.T.,.F.,(4,2,2,2,2,2,2,2,2,2,2,2,
2,2,2,2,4),(0.,0.0946120580087934,0.189224116017587,0.283822945575014,0.378421775132442,
0.47302060468987,0.567619434247297,0.66223149225609,0.756843550264884,0.851455608273677,
0.94606766628247,1.0406664958399,1.13526532539733,1.22986415495475,1.32446298451218,
1.41907504252097,1.51368710052977),.UNSPECIFIED.);
#189=B_SPLINE_CURVE_WITH_KNOTS('',3,(#8743,#8744,#8745,#8746,#8747,#8748,
#8749,#8750,#8751,#8752),.UNSPECIFIED.,.F.,.F.,(4,2,2,2,4),(1.13193471301885,
1.22626174930539,1.32058878559194,1.41491753480854,1.50924628402513),
 .UNSPECIFIED.);
#190=B_SPLINE_CURVE_WITH_KNOTS('',3,(#8754,#8755,#8756,#8757,#8758,#8759,
#8760,#8761,#8762,#8763,#8764,#8765,#8766,#8767,#8768,#8769,#8770,#8771),
 .UNSPECIFIED.,.F.,.F.,(4,2,2,2,2,2,2,2,4),(0.377311571006283,0.47163860729283,
0.565965643579376,0.660294392795971,0.754623142012565,0.84895189122916,
0.943280640445755,1.0376076767323,1.13193471301885),.UNSPECIFIED.);
#191=B_SPLINE_CURVE_WITH_KNOTS('',3,(#8772,#8773,#8774,#8775,#8776,#8777,
#8778,#8779,#8780,#8781),.UNSPECIFIED.,.F.,.F.,(4,2,2,2,4),(1.50924628402513,
1.60357503324173,1.69790378245832,1.79223081874487,1.88655785503141),
 .UNSPECIFIED.);
#192=B_SPLINE_CURVE_WITH_KNOTS('',3,(#8790,#8791,#8792,#8793,#8794,#8795,
#8796,#8797,#8798,#8799,#8800,#8801,#8802,#8803,#8804,#8805,#8806,#8807),
 .UNSPECIFIED.,.F.,.F.,(4,2,2,2,2,2,2,2,4),(0.377311571006282,0.471638607292829,
0.565965643579376,0.660294392795971,0.754623142012565,0.84895189122916,
0.943280640445754,1.0376076767323,1.13193471301885),.UNSPECIFIED.);
#193=B_SPLINE_CURVE_WITH_KNOTS('',3,(#8809,#8810,#8811,#8812,#8813,#8814,
#8815,#8816,#8817,#8818),.UNSPECIFIED.,.F.,.F.,(4,2,2,2,4),(1.13193471301885,
1.22626174930539,1.32058878559194,1.41491753480854,1.50924628402513),
 .UNSPECIFIED.);
#194=B_SPLINE_CURVE_WITH_KNOTS('',3,(#8819,#8820,#8821,#8822,#8823,#8824,
#8825,#8826,#8827,#8828),.UNSPECIFIED.,.F.,.F.,(4,2,2,2,4),(1.50924628402513,
1.60357503324172,1.69790378245832,1.79223081874487,1.88655785503141),
 .UNSPECIFIED.);
#195=B_SPLINE_CURVE_WITH_KNOTS('',3,(#8831,#8832,#8833,#8834,#8835,#8836,
#8837,#8838,#8839,#8840,#8841,#8842,#8843,#8844,#8845,#8846,#8847,#8848),
 .UNSPECIFIED.,.F.,.F.,(4,2,2,2,2,2,2,2,4),(0.377311571006283,0.47163860729283,
0.565965643579376,0.660294392795971,0.754623142012565,0.84895189122916,
0.943280640445754,1.0376076767323,1.13193471301885),.UNSPECIFIED.);
#196=B_SPLINE_CURVE_WITH_KNOTS('',3,(#8850,#8851,#8852,#8853,#8854,#8855,
#8856,#8857,#8858,#8859),.UNSPECIFIED.,.F.,.F.,(4,2,2,2,4),(1.13193471301885,
1.22626174930539,1.32058878559194,1.41491753480854,1.50924628402513),
 .UNSPECIFIED.);
#197=B_SPLINE_CURVE_WITH_KNOTS('',3,(#8860,#8861,#8862,#8863,#8864,#8865,
#8866,#8867,#8868,#8869),.UNSPECIFIED.,.F.,.F.,(4,2,2,2,4),(1.50924628402513,
1.60357503324173,1.69790378245832,1.79223081874487,1.88655785503141),
 .UNSPECIFIED.);
#198=B_SPLINE_CURVE_WITH_KNOTS('',3,(#8872,#8873,#8874,#8875,#8876,#8877,
#8878,#8879,#8880,#8881,#8882,#8883,#8884,#8885,#8886,#8887,#8888,#8889),
 .UNSPECIFIED.,.F.,.F.,(4,2,2,2,2,2,2,2,4),(0.377311571006282,0.471638607292829,
0.565965643579376,0.66029439279597,0.754623142012565,0.84895189122916,0.943280640445754,
1.0376076767323,1.13193471301885),.UNSPECIFIED.);
#199=B_SPLINE_CURVE_WITH_KNOTS('',3,(#8891,#8892,#8893,#8894,#8895,#8896,
#8897,#8898,#8899,#8900),.UNSPECIFIED.,.F.,.F.,(4,2,2,2,4),(1.13193471301885,
1.22626174930539,1.32058878559194,1.41491753480854,1.50924628402513),
 .UNSPECIFIED.);
#200=B_SPLINE_CURVE_WITH_KNOTS('',3,(#8901,#8902,#8903,#8904,#8905,#8906,
#8907,#8908,#8909,#8910),.UNSPECIFIED.,.F.,.F.,(4,2,2,2,4),(1.50924628402513,
1.60357503324172,1.69790378245832,1.79223081874487,1.88655785503141),
 .UNSPECIFIED.);
#201=B_SPLINE_CURVE_WITH_KNOTS('',3,(#8913,#8914,#8915,#8916,#8917,#8918,
#8919,#8920,#8921,#8922,#8923,#8924,#8925,#8926,#8927,#8928,#8929,#8930),
 .UNSPECIFIED.,.F.,.F.,(4,2,2,2,2,2,2,2,4),(0.377311571006283,0.471638607292829,
0.565965643579376,0.660294392795971,0.754623142012565,0.84895189122916,
0.943280640445755,1.0376076767323,1.13193471301885),.UNSPECIFIED.);
#202=B_SPLINE_CURVE_WITH_KNOTS('',3,(#8932,#8933,#8934,#8935,#8936,#8937,
#8938,#8939,#8940,#8941),.UNSPECIFIED.,.F.,.F.,(4,2,2,2,4),(1.13193471301885,
1.22626174930539,1.32058878559194,1.41491753480854,1.50924628402513),
 .UNSPECIFIED.);
#203=B_SPLINE_CURVE_WITH_KNOTS('',3,(#8942,#8943,#8944,#8945,#8946,#8947,
#8948,#8949,#8950,#8951),.UNSPECIFIED.,.F.,.F.,(4,2,2,2,4),(1.50924628402513,
1.60357503324172,1.69790378245832,1.79223081874487,1.88655785503141),
 .UNSPECIFIED.);
#204=B_SPLINE_CURVE_WITH_KNOTS('',3,(#8955,#8956,#8957,#8958,#8959,#8960,
#8961,#8962,#8963,#8964,#8965,#8966,#8967,#8968,#8969,#8970,#8971,#8972,
#8973,#8974,#8975,#8976,#8977,#8978,#8979,#8980,#8981,#8982,#8983,#8984,
#8985,#8986,#8987,#8988),.UNSPECIFIED.,.T.,.F.,(4,2,2,2,2,2,2,2,2,2,2,2,
2,2,2,2,4),(0.,0.0946120580087934,0.189224116017587,0.283822945575014,0.378421775132442,
0.47302060468987,0.567619434247297,0.66223149225609,0.756843550264884,0.851455608273677,
0.94606766628247,1.0406664958399,1.13526532539733,1.22986415495475,1.32446298451218,
1.41907504252097,1.51368710052977),.UNSPECIFIED.);
#205=B_SPLINE_CURVE_WITH_KNOTS('',3,(#8991,#8992,#8993,#8994,#8995,#8996,
#8997,#8998,#8999,#9000,#9001,#9002,#9003,#9004,#9005,#9006,#9007,#9008,
#9009,#9010,#9011,#9012,#9013,#9014,#9015,#9016,#9017,#9018,#9019,#9020,
#9021,#9022,#9023,#9024),.UNSPECIFIED.,.T.,.F.,(4,2,2,2,2,2,2,2,2,2,2,2,
2,2,2,2,4),(0.,0.0946120580087934,0.189224116017587,0.283822945575014,0.378421775132442,
0.47302060468987,0.567619434247297,0.66223149225609,0.756843550264884,0.851455608273677,
0.94606766628247,1.0406664958399,1.13526532539733,1.22986415495475,1.32446298451218,
1.41907504252097,1.51368710052977),.UNSPECIFIED.);
#206=B_SPLINE_CURVE_WITH_KNOTS('',3,(#9029,#9030,#9031,#9032,#9033,#9034,
#9035,#9036,#9037,#9038,#9039,#9040,#9041,#9042,#9043,#9044,#9045,#9046,
#9047,#9048,#9049,#9050,#9051,#9052,#9053,#9054,#9055,#9056,#9057,#9058,
#9059,#9060,#9061,#9062),.UNSPECIFIED.,.T.,.F.,(4,2,2,2,2,2,2,2,2,2,2,2,
2,2,2,2,4),(0.,0.0946120580087934,0.189224116017587,0.283822945575014,0.378421775132442,
0.47302060468987,0.567619434247297,0.66223149225609,0.756843550264884,0.851455608273677,
0.94606766628247,1.0406664958399,1.13526532539733,1.22986415495475,1.32446298451218,
1.41907504252097,1.51368710052977),.UNSPECIFIED.);
#207=B_SPLINE_CURVE_WITH_KNOTS('',3,(#9065,#9066,#9067,#9068,#9069,#9070,
#9071,#9072,#9073,#9074,#9075,#9076,#9077,#9078,#9079,#9080,#9081,#9082,
#9083,#9084,#9085,#9086,#9087,#9088,#9089,#9090,#9091,#9092,#9093,#9094,
#9095,#9096,#9097,#9098),.UNSPECIFIED.,.T.,.F.,(4,2,2,2,2,2,2,2,2,2,2,2,
2,2,2,2,4),(0.,0.0946120580087934,0.189224116017587,0.283822945575014,0.378421775132442,
0.47302060468987,0.567619434247297,0.66223149225609,0.756843550264884,0.851455608273677,
0.94606766628247,1.0406664958399,1.13526532539733,1.22986415495475,1.32446298451218,
1.41907504252097,1.51368710052977),.UNSPECIFIED.);
#208=B_SPLINE_CURVE_WITH_KNOTS('',3,(#9411,#9412,#9413,#9414,#9415,#9416,
#9417,#9418,#9419,#9420),.UNSPECIFIED.,.F.,.F.,(4,2,2,2,4),(0.803821788694082,
0.87295099185362,0.95230721290097,1.03166343394832,1.10079263710786),
 .UNSPECIFIED.);
#209=B_SPLINE_CURVE_WITH_KNOTS('',3,(#9426,#9427,#9428,#9429,#9430,#9431,
#9432,#9433,#9434,#9435,#9436,#9437,#9438,#9439,#9440,#9441,#9442,#9443),
 .UNSPECIFIED.,.F.,.F.,(4,2,2,2,2,2,2,2,4),(0.,0.0791670250779307,0.158334050155861,
0.237500747381213,0.316667444606564,0.395834141831916,0.475000839057267,
0.554167864135198,0.633334889213129),.UNSPECIFIED.);
#210=B_SPLINE_CURVE_WITH_KNOTS('',3,(#9444,#9445,#9446,#9447,#9448,#9449,
#9450,#9451,#9452,#9453,#9454,#9455,#9456,#9457,#9458,#9459,#9460,#9461),
 .UNSPECIFIED.,.F.,.F.,(4,2,2,2,2,2,2,2,4),(0.633334889213129,0.712501914291059,
0.79166893936899,0.870835636594341,0.950002333819693,1.02916903104504,1.1083357282704,
1.18750275334833,1.26666977842626),.UNSPECIFIED.);
#211=B_SPLINE_CURVE_WITH_KNOTS('',3,(#9464,#9465,#9466,#9467,#9468,#9469,
#9470,#9471,#9472,#9473),.UNSPECIFIED.,.F.,.F.,(4,2,2,2,4),(0.168950313426771,
0.238079516586307,0.317435737633657,0.396791958681006,0.465921161840543),
 .UNSPECIFIED.);
#212=B_SPLINE_CURVE_WITH_KNOTS('',3,(#9516,#9517,#9518,#9519,#9520,#9521,
#9522,#9523,#9524,#9525,#9526,#9527,#9528,#9529),.UNSPECIFIED.,.F.,.F.,
(4,2,2,2,2,2,4),(0.75600573798702,0.793568827564647,0.872922520054201,0.952276212543756,
1.03162990503331,1.11098359752287,1.14854668710049),.UNSPECIFIED.);
#213=B_SPLINE_CURVE_WITH_KNOTS('',3,(#9535,#9536,#9537,#9538,#9539,#9540,
#9541,#9542,#9543,#9544,#9545,#9546,#9547,#9548,#9549,#9550,#9551,#9552),
 .UNSPECIFIED.,.F.,.F.,(4,2,2,2,2,2,2,2,4),(0.,0.079216580773363,0.158433161546726,
0.23764869707457,0.316864232602414,0.396079768130259,0.475295303658103,
0.554511884431466,0.633728465204829),.UNSPECIFIED.);
#214=B_SPLINE_CURVE_WITH_KNOTS('',3,(#9553,#9554,#9555,#9556,#9557,#9558,
#9559,#9560,#9561,#9562,#9563,#9564,#9565,#9566,#9567,#9568,#9569,#9570),
 .UNSPECIFIED.,.F.,.F.,(4,2,2,2,2,2,2,2,4),(0.633728465204829,0.712945045978192,
0.792161626751555,0.871377162279399,0.950592697807244,1.02980823333509,
1.10902376886293,1.18824034963629,1.26745693040966),.UNSPECIFIED.);
#215=B_SPLINE_CURVE_WITH_KNOTS('',3,(#9573,#9574,#9575,#9576,#9577,#9578,
#9579,#9580,#9581,#9582,#9583,#9584,#9585,#9586),.UNSPECIFIED.,.F.,.F.,
(4,2,2,2,2,2,4),(0.121154929624515,0.158718019202143,0.238071711691697,
0.317425404181252,0.396779096670807,0.476132789160362,0.513695878737989),
 .UNSPECIFIED.);
#216=B_SPLINE_CURVE_WITH_KNOTS('',3,(#9611,#9612,#9613,#9614,#9615,#9616,
#9617,#9618,#9619,#9620,#9621,#9622,#9623,#9624),.UNSPECIFIED.,.F.,.F.,
(4,2,2,2,2,2,4),(0.756005737987019,0.793568827564645,0.8729225200542,0.952276212543755,
1.03162990503331,1.11098359752287,1.14854668710049),.UNSPECIFIED.);
#217=B_SPLINE_CURVE_WITH_KNOTS('',3,(#9630,#9631,#9632,#9633,#9634,#9635,
#9636,#9637,#9638,#9639,#9640,#9641,#9642,#9643,#9644,#9645,#9646,#9647),
 .UNSPECIFIED.,.F.,.F.,(4,2,2,2,2,2,2,2,4),(0.,0.0792165807733624,0.158433161546725,
0.237648697074569,0.316864232602414,0.396079768130259,0.475295303658103,
0.554511884431466,0.633728465204828),.UNSPECIFIED.);
#218=B_SPLINE_CURVE_WITH_KNOTS('',3,(#9648,#9649,#9650,#9651,#9652,#9653,
#9654,#9655,#9656,#9657,#9658,#9659,#9660,#9661,#9662,#9663,#9664,#9665),
 .UNSPECIFIED.,.F.,.F.,(4,2,2,2,2,2,2,2,4),(0.633728465204828,0.712945045978191,
0.792161626751553,0.871377162279398,0.950592697807242,1.02980823333509,
1.10902376886293,1.18824034963629,1.26745693040966),.UNSPECIFIED.);
#219=B_SPLINE_CURVE_WITH_KNOTS('',3,(#9668,#9669,#9670,#9671,#9672,#9673,
#9674,#9675,#9676,#9677,#9678,#9679,#9680,#9681),.UNSPECIFIED.,.F.,.F.,
(4,2,2,2,2,2,4),(0.121154929624521,0.158718019202141,0.238071711691696,
0.317425404181252,0.396779096670807,0.476132789160362,0.513695878737985),
 .UNSPECIFIED.);
#220=B_SPLINE_CURVE_WITH_KNOTS('',3,(#9730,#9731,#9732,#9733,#9734,#9735,
#9736,#9737,#9738,#9739,#9740,#9741,#9742,#9743,#9744,#9745,#9746,#9747),
 .UNSPECIFIED.,.F.,.F.,(4,2,2,2,2,2,2,2,4),(0.,0.0472365751919841,0.0944731503839683,
0.14170659898184,0.188940047579712,0.236173496177583,0.283406944775455,
0.330643519967439,0.377880095159423),.UNSPECIFIED.);
#221=B_SPLINE_CURVE_WITH_KNOTS('',3,(#9748,#9749,#9750,#9751,#9752,#9753,
#9754,#9755,#9756,#9757,#9758,#9759,#9760,#9761,#9762,#9763,#9764,#9765),
 .UNSPECIFIED.,.F.,.F.,(4,2,2,2,2,2,2,2,4),(0.377880095159423,0.425116670351408,
0.472353245543392,0.519586694141263,0.566820142739135,0.614053591337007,
0.661287039934879,0.708523615126863,0.755760190318847),.UNSPECIFIED.);
#222=B_SPLINE_CURVE_WITH_KNOTS('',3,(#9768,#9769,#9770,#9771,#9772,#9773,
#9774,#9775,#9776,#9777,#9778,#9779,#9780,#9781,#9782,#9783,#9784,#9785),
 .UNSPECIFIED.,.F.,.F.,(4,2,2,2,2,2,2,2,4),(0.,0.0472365751919841,0.0944731503839682,
0.14170659898184,0.188940047579712,0.236173496177583,0.283406944775455,
0.330643519967439,0.377880095159423),.UNSPECIFIED.);
#223=B_SPLINE_CURVE_WITH_KNOTS('',3,(#9786,#9787,#9788,#9789,#9790,#9791,
#9792,#9793,#9794,#9795,#9796,#9797,#9798,#9799,#9800,#9801,#9802,#9803),
 .UNSPECIFIED.,.F.,.F.,(4,2,2,2,2,2,2,2,4),(0.377880095159423,0.425116670351408,
0.472353245543392,0.519586694141263,0.566820142739135,0.614053591337007,
0.661287039934879,0.708523615126863,0.755760190318847),.UNSPECIFIED.);
#224=B_SPLINE_CURVE_WITH_KNOTS('',3,(#9806,#9807,#9808,#9809,#9810,#9811,
#9812,#9813,#9814,#9815,#9816,#9817,#9818,#9819,#9820,#9821,#9822,#9823),
 .UNSPECIFIED.,.F.,.F.,(4,2,2,2,2,2,2,2,4),(0.,0.0472365751919841,0.0944731503839683,
0.14170659898184,0.188940047579712,0.236173496177583,0.283406944775455,
0.330643519967439,0.377880095159423),.UNSPECIFIED.);
#225=B_SPLINE_CURVE_WITH_KNOTS('',3,(#9824,#9825,#9826,#9827,#9828,#9829,
#9830,#9831,#9832,#9833,#9834,#9835,#9836,#9837,#9838,#9839,#9840,#9841),
 .UNSPECIFIED.,.F.,.F.,(4,2,2,2,2,2,2,2,4),(0.377880095159423,0.425116670351408,
0.472353245543392,0.519586694141263,0.566820142739135,0.614053591337007,
0.661287039934879,0.708523615126863,0.755760190318847),.UNSPECIFIED.);
#226=B_SPLINE_CURVE_WITH_KNOTS('',3,(#9845,#9846,#9847,#9848,#9849,#9850,
#9851,#9852,#9853,#9854),.UNSPECIFIED.,.F.,.F.,(4,2,2,2,4),(0.565665723963061,
0.61280433739166,0.659942950820258,0.70708195805217,0.754220965284082),
 .UNSPECIFIED.);
#227=B_SPLINE_CURVE_WITH_KNOTS('',3,(#9856,#9857,#9858,#9859,#9860,#9861,
#9862,#9863,#9864,#9865,#9866,#9867,#9868,#9869,#9870,#9871,#9872,#9873),
 .UNSPECIFIED.,.F.,.F.,(4,2,2,2,2,2,2,2,4),(0.18855524132102,0.235693854749619,
0.282832468178217,0.329971475410129,0.377110482642041,0.424249489873953,
0.471388497105864,0.518527110534463,0.565665723963061),.UNSPECIFIED.);
#228=B_SPLINE_CURVE_WITH_KNOTS('',3,(#9874,#9875,#9876,#9877,#9878,#9879,
#9880,#9881,#9882,#9883),.UNSPECIFIED.,.F.,.F.,(4,2,2,2,4),(0.754220965284082,
0.801359972515993,0.848498979747905,0.895637593176504,0.942776206605102),
 .UNSPECIFIED.);
#229=B_SPLINE_CURVE_WITH_KNOTS('',3,(#9889,#9890,#9891,#9892,#9893,#9894,
#9895,#9896,#9897,#9898),.UNSPECIFIED.,.F.,.F.,(4,2,2,2,4),(0.565665723963061,
0.61280433739166,0.659942950820258,0.70708195805217,0.754220965284082),
 .UNSPECIFIED.);
#230=B_SPLINE_CURVE_WITH_KNOTS('',3,(#9900,#9901,#9902,#9903,#9904,#9905,
#9906,#9907,#9908,#9909,#9910,#9911,#9912,#9913,#9914,#9915,#9916,#9917),
 .UNSPECIFIED.,.F.,.F.,(4,2,2,2,2,2,2,2,4),(0.18855524132102,0.235693854749619,
0.282832468178217,0.329971475410129,0.377110482642041,0.424249489873953,
0.471388497105864,0.518527110534463,0.565665723963061),.UNSPECIFIED.);
#231=B_SPLINE_CURVE_WITH_KNOTS('',3,(#9918,#9919,#9920,#9921,#9922,#9923,
#9924,#9925,#9926,#9927),.UNSPECIFIED.,.F.,.F.,(4,2,2,2,4),(0.754220965284082,
0.801359972515993,0.848498979747905,0.895637593176504,0.942776206605102),
 .UNSPECIFIED.);
#232=B_SPLINE_CURVE_WITH_KNOTS('',3,(#9937,#9938,#9939,#9940,#9941,#9942,
#9943,#9944,#9945,#9946,#9947,#9948,#9949,#9950,#9951,#9952,#9953,#9954),
 .UNSPECIFIED.,.F.,.F.,(4,2,2,2,2,2,2,2,4),(0.18855524132102,0.235693854749619,
0.282832468178217,0.329971475410129,0.377110482642041,0.424249489873953,
0.471388497105864,0.518527110534463,0.565665723963061),.UNSPECIFIED.);
#233=B_SPLINE_CURVE_WITH_KNOTS('',3,(#9956,#9957,#9958,#9959,#9960,#9961,
#9962,#9963,#9964,#9965),.UNSPECIFIED.,.F.,.F.,(4,2,2,2,4),(0.565665723963061,
0.61280433739166,0.659942950820258,0.70708195805217,0.754220965284082),
 .UNSPECIFIED.);
#234=B_SPLINE_CURVE_WITH_KNOTS('',3,(#9966,#9967,#9968,#9969,#9970,#9971,
#9972,#9973,#9974,#9975),.UNSPECIFIED.,.F.,.F.,(4,2,2,2,4),(0.754220965284082,
0.801359972515993,0.848498979747905,0.895637593176504,0.942776206605102),
 .UNSPECIFIED.);
#235=B_SPLINE_CURVE_WITH_KNOTS('',3,(#9978,#9979,#9980,#9981,#9982,#9983,
#9984,#9985,#9986,#9987,#9988,#9989,#9990,#9991,#9992,#9993,#9994,#9995),
 .UNSPECIFIED.,.F.,.F.,(4,2,2,2,2,2,2,2,4),(0.18855524132102,0.235693854749619,
0.282832468178217,0.329971475410129,0.377110482642041,0.424249489873953,
0.471388497105864,0.518527110534463,0.565665723963061),.UNSPECIFIED.);
#236=B_SPLINE_CURVE_WITH_KNOTS('',3,(#9997,#9998,#9999,#10000,#10001,#10002,
#10003,#10004,#10005,#10006),.UNSPECIFIED.,.F.,.F.,(4,2,2,2,4),(0.565665723963061,
0.61280433739166,0.659942950820258,0.70708195805217,0.754220965284082),
 .UNSPECIFIED.);
#237=B_SPLINE_CURVE_WITH_KNOTS('',3,(#10007,#10008,#10009,#10010,#10011,
#10012,#10013,#10014,#10015,#10016),.UNSPECIFIED.,.F.,.F.,(4,2,2,2,4),(0.754220965284082,
0.801359972515993,0.848498979747905,0.895637593176504,0.942776206605102),
 .UNSPECIFIED.);
#238=SPHERICAL_SURFACE('',#5956,2.35);
#239=SPHERICAL_SURFACE('',#5996,2.35);
#240=SHAPE_REPRESENTATION_RELATIONSHIP('SRR','None',#10926,#265);
#241=SHAPE_REPRESENTATION_RELATIONSHIP('SRR','None',#10927,#266);
#242=SHAPE_REPRESENTATION_RELATIONSHIP('SRR','None',#10928,#267);
#243=SHAPE_REPRESENTATION_RELATIONSHIP('SRR','None',#10929,#268);
#244=SHAPE_REPRESENTATION_RELATIONSHIP('SRR','None',#10930,#269);
#245=SHAPE_REPRESENTATION_RELATIONSHIP('SRR','None',#10931,#270);
#246=SHAPE_REPRESENTATION_RELATIONSHIP('SRR','None',#10932,#271);
#247=SHAPE_REPRESENTATION_RELATIONSHIP('SRR','None',#10934,#272);
#248=SHAPE_REPRESENTATION_RELATIONSHIP('SRR','None',#10935,#273);
#249=SHAPE_REPRESENTATION_RELATIONSHIP('SRR','None',#10936,#274);
#250=SHAPE_REPRESENTATION_RELATIONSHIP('SRR','None',#10937,#275);
#251=SHAPE_REPRESENTATION_RELATIONSHIP('SRR','None',#10939,#276);
#252=SHAPE_REPRESENTATION_RELATIONSHIP('SRR','None',#10940,#277);
#253=SHAPE_REPRESENTATION_RELATIONSHIP('SRR','None',#10941,#278);
#254=SHAPE_REPRESENTATION_RELATIONSHIP('SRR','None',#10942,#279);
#255=SHAPE_REPRESENTATION_RELATIONSHIP('SRR','None',#10943,#280);
#256=SHAPE_REPRESENTATION_RELATIONSHIP('SRR','None',#10944,#281);
#257=SHAPE_REPRESENTATION_RELATIONSHIP('SRR','None',#10945,#282);
#258=SHAPE_REPRESENTATION_RELATIONSHIP('SRR','None',#10946,#283);
#259=SHAPE_REPRESENTATION_RELATIONSHIP('SRR','None',#10947,#284);
#260=SHAPE_REPRESENTATION_RELATIONSHIP('SRR','None',#10948,#285);
#261=SHAPE_REPRESENTATION_RELATIONSHIP('SRR','None',#10949,#286);
#262=SHAPE_REPRESENTATION_RELATIONSHIP('SRR','None',#10950,#287);
#263=SHAPE_REPRESENTATION_RELATIONSHIP('SRR','None',#10951,#288);
#264=SHAPE_REPRESENTATION_RELATIONSHIP('SRR','None',#10952,#289);
#265=ADVANCED_BREP_SHAPE_REPRESENTATION('',(#316),#10794);
#266=ADVANCED_BREP_SHAPE_REPRESENTATION('',(#317),#10795);
#267=ADVANCED_BREP_SHAPE_REPRESENTATION('',(#318),#10796);
#268=ADVANCED_BREP_SHAPE_REPRESENTATION('',(#319),#10797);
#269=ADVANCED_BREP_SHAPE_REPRESENTATION('',(#320),#10798);
#270=ADVANCED_BREP_SHAPE_REPRESENTATION('',(#321),#10799);
#271=ADVANCED_BREP_SHAPE_REPRESENTATION('',(#322),#10800);
#272=ADVANCED_BREP_SHAPE_REPRESENTATION('',(#323),#10802);
#273=ADVANCED_BREP_SHAPE_REPRESENTATION('',(#324,#325),#10803);
#274=ADVANCED_BREP_SHAPE_REPRESENTATION('',(#326),#10804);
#275=ADVANCED_BREP_SHAPE_REPRESENTATION('',(#22),#10805);
#276=ADVANCED_BREP_SHAPE_REPRESENTATION('',(#327),#10807);
#277=ADVANCED_BREP_SHAPE_REPRESENTATION('',(#328),#10808);
#278=ADVANCED_BREP_SHAPE_REPRESENTATION('',(#329),#10809);
#279=ADVANCED_BREP_SHAPE_REPRESENTATION('',(#330),#10810);
#280=ADVANCED_BREP_SHAPE_REPRESENTATION('',(#331),#10811);
#281=ADVANCED_BREP_SHAPE_REPRESENTATION('',(#332),#10812);
#282=ADVANCED_BREP_SHAPE_REPRESENTATION('',(#333),#10813);
#283=ADVANCED_BREP_SHAPE_REPRESENTATION('',(#334),#10814);
#284=ADVANCED_BREP_SHAPE_REPRESENTATION('',(#335),#10815);
#285=ADVANCED_BREP_SHAPE_REPRESENTATION('',(#336),#10816);
#286=ADVANCED_BREP_SHAPE_REPRESENTATION('',(#337),#10817);
#287=ADVANCED_BREP_SHAPE_REPRESENTATION('',(#23),#10818);
#288=ADVANCED_BREP_SHAPE_REPRESENTATION('',(#338),#10819);
#289=ADVANCED_BREP_SHAPE_REPRESENTATION('',(#339),#10820);
#290=STYLED_ITEM('',(#11114),#316);
#291=STYLED_ITEM('',(#11149),#317);
#292=STYLED_ITEM('',(#11149),#318);
#293=STYLED_ITEM('',(#11128),#319);
#294=STYLED_ITEM('',(#11128),#320);
#295=STYLED_ITEM('',(#11128),#321);
#296=STYLED_ITEM('',(#11128),#322);
#297=STYLED_ITEM('',(#11114),#323);
#298=STYLED_ITEM('',(#11135),#324);
#299=STYLED_ITEM('',(#11135),#325);
#300=STYLED_ITEM('',(#11142),#326);
#301=STYLED_ITEM('',(#11142),#22);
#302=STYLED_ITEM('',(#11135),#327);
#303=STYLED_ITEM('',(#11149),#328);
#304=STYLED_ITEM('',(#11121),#329);
#305=STYLED_ITEM('',(#11128),#330);
#306=STYLED_ITEM('',(#11149),#331);
#307=STYLED_ITEM('',(#11149),#332);
#308=STYLED_ITEM('',(#11149),#333);
#309=STYLED_ITEM('',(#11135),#334);
#310=STYLED_ITEM('',(#11135),#335);
#311=STYLED_ITEM('',(#11128),#336);
#312=STYLED_ITEM('',(#11135),#337);
#313=STYLED_ITEM('',(#11142),#23);
#314=STYLED_ITEM('',(#11135),#338);
#315=STYLED_ITEM('',(#11142),#339);
#316=MANIFOLD_SOLID_BREP('Body1',#5573);
#317=MANIFOLD_SOLID_BREP('Body1',#5574);
#318=MANIFOLD_SOLID_BREP('Body1',#5575);
#319=MANIFOLD_SOLID_BREP('Body1',#5576);
#320=MANIFOLD_SOLID_BREP('Body1',#5577);
#321=MANIFOLD_SOLID_BREP('Body1',#5578);
#322=MANIFOLD_SOLID_BREP('Body1',#5579);
#323=MANIFOLD_SOLID_BREP('Body1',#5580);
#324=MANIFOLD_SOLID_BREP('Body1',#5581);
#325=MANIFOLD_SOLID_BREP('Body2',#5582);
#326=MANIFOLD_SOLID_BREP('Body1',#5583);
#327=MANIFOLD_SOLID_BREP('Body1',#5586);
#328=MANIFOLD_SOLID_BREP('Body1',#5587);
#329=MANIFOLD_SOLID_BREP('Body1',#5588);
#330=MANIFOLD_SOLID_BREP('Body1',#5589);
#331=MANIFOLD_SOLID_BREP('Body1',#5590);
#332=MANIFOLD_SOLID_BREP('Body1',#5591);
#333=MANIFOLD_SOLID_BREP('Body1',#5592);
#334=MANIFOLD_SOLID_BREP('Body1',#5593);
#335=MANIFOLD_SOLID_BREP('Body1',#5594);
#336=MANIFOLD_SOLID_BREP('Body1',#5595);
#337=MANIFOLD_SOLID_BREP('Body1',#5596);
#338=MANIFOLD_SOLID_BREP('Body1',#5599);
#339=MANIFOLD_SOLID_BREP('Body1',#5600);
#340=FACE_BOUND('',#911,.T.);
#341=FACE_BOUND('',#912,.T.);
#342=FACE_BOUND('',#913,.T.);
#343=FACE_BOUND('',#914,.T.);
#344=FACE_BOUND('',#916,.T.);
#345=FACE_BOUND('',#917,.T.);
#346=FACE_BOUND('',#918,.T.);
#347=FACE_BOUND('',#919,.T.);
#348=FACE_BOUND('',#935,.T.);
#349=FACE_BOUND('',#937,.T.);
#350=FACE_BOUND('',#941,.T.);
#351=FACE_BOUND('',#943,.T.);
#352=FACE_BOUND('',#947,.T.);
#353=FACE_BOUND('',#949,.T.);
#354=FACE_BOUND('',#953,.T.);
#355=FACE_BOUND('',#955,.T.);
#356=FACE_BOUND('',#959,.T.);
#357=FACE_BOUND('',#960,.T.);
#358=FACE_BOUND('',#968,.T.);
#359=FACE_BOUND('',#969,.T.);
#360=FACE_BOUND('',#970,.T.);
#361=FACE_BOUND('',#973,.T.);
#362=FACE_BOUND('',#975,.T.);
#363=FACE_BOUND('',#988,.T.);
#364=FACE_BOUND('',#989,.T.);
#365=FACE_BOUND('',#990,.T.);
#366=FACE_BOUND('',#993,.T.);
#367=FACE_BOUND('',#995,.T.);
#368=FACE_BOUND('',#996,.T.);
#369=FACE_BOUND('',#998,.T.);
#370=FACE_BOUND('',#1002,.T.);
#371=FACE_BOUND('',#1003,.T.);
#372=FACE_BOUND('',#1004,.T.);
#373=FACE_BOUND('',#1005,.T.);
#374=FACE_BOUND('',#1006,.T.);
#375=FACE_BOUND('',#1007,.T.);
#376=FACE_BOUND('',#1013,.T.);
#377=FACE_BOUND('',#1015,.T.);
#378=FACE_BOUND('',#1018,.T.);
#379=FACE_BOUND('',#1020,.T.);
#380=FACE_BOUND('',#1021,.T.);
#381=FACE_BOUND('',#1022,.T.);
#382=FACE_BOUND('',#1023,.T.);
#383=FACE_BOUND('',#1024,.T.);
#384=FACE_BOUND('',#1025,.T.);
#385=FACE_BOUND('',#1029,.T.);
#386=FACE_BOUND('',#1031,.T.);
#387=FACE_BOUND('',#1046,.T.);
#388=FACE_BOUND('',#1069,.T.);
#389=FACE_BOUND('',#1071,.T.);
#390=FACE_BOUND('',#1073,.T.);
#391=FACE_BOUND('',#1075,.T.);
#392=FACE_BOUND('',#1077,.T.);
#393=FACE_BOUND('',#1079,.T.);
#394=FACE_BOUND('',#1081,.T.);
#395=FACE_BOUND('',#1085,.T.);
#396=FACE_BOUND('',#1087,.T.);
#397=FACE_BOUND('',#1091,.T.);
#398=FACE_BOUND('',#1093,.T.);
#399=FACE_BOUND('',#1097,.T.);
#400=FACE_BOUND('',#1099,.T.);
#401=FACE_BOUND('',#1103,.T.);
#402=FACE_BOUND('',#1105,.T.);
#403=FACE_BOUND('',#1109,.T.);
#404=FACE_BOUND('',#1111,.T.);
#405=FACE_BOUND('',#1119,.T.);
#406=FACE_BOUND('',#1121,.T.);
#407=FACE_BOUND('',#1123,.T.);
#408=FACE_BOUND('',#1125,.T.);
#409=FACE_BOUND('',#1130,.T.);
#410=FACE_BOUND('',#1132,.T.);
#411=FACE_BOUND('',#1134,.T.);
#412=FACE_BOUND('',#1136,.T.);
#413=FACE_BOUND('',#1141,.T.);
#414=FACE_BOUND('',#1143,.T.);
#415=FACE_BOUND('',#1145,.T.);
#416=FACE_BOUND('',#1147,.T.);
#417=FACE_BOUND('',#1150,.T.);
#418=FACE_BOUND('',#1153,.T.);
#419=FACE_BOUND('',#1155,.T.);
#420=FACE_BOUND('',#1156,.T.);
#421=FACE_BOUND('',#1157,.T.);
#422=FACE_BOUND('',#1161,.T.);
#423=FACE_BOUND('',#1162,.T.);
#424=FACE_BOUND('',#1163,.T.);
#425=FACE_BOUND('',#1167,.T.);
#426=FACE_BOUND('',#1169,.T.);
#427=FACE_BOUND('',#1172,.T.);
#428=FACE_BOUND('',#1174,.T.);
#429=FACE_BOUND('',#1271,.T.);
#430=FACE_BOUND('',#1302,.T.);
#431=PLANE('',#5892);
#432=PLANE('',#5893);
#433=PLANE('',#5894);
#434=PLANE('',#5895);
#435=PLANE('',#5896);
#436=PLANE('',#5897);
#437=PLANE('',#5899);
#438=PLANE('',#5900);
#439=PLANE('',#5901);
#440=PLANE('',#5902);
#441=PLANE('',#5903);
#442=PLANE('',#5904);
#443=PLANE('',#5906);
#444=PLANE('',#5907);
#445=PLANE('',#5908);
#446=PLANE('',#5909);
#447=PLANE('',#5910);
#448=PLANE('',#5911);
#449=PLANE('',#5919);
#450=PLANE('',#5920);
#451=PLANE('',#5928);
#452=PLANE('',#5929);
#453=PLANE('',#5937);
#454=PLANE('',#5938);
#455=PLANE('',#5946);
#456=PLANE('',#5947);
#457=PLANE('',#5958);
#458=PLANE('',#5960);
#459=PLANE('',#5962);
#460=PLANE('',#5964);
#461=PLANE('',#5965);
#462=PLANE('',#5967);
#463=PLANE('',#5968);
#464=PLANE('',#5974);
#465=PLANE('',#5975);
#466=PLANE('',#5976);
#467=PLANE('',#5977);
#468=PLANE('',#5978);
#469=PLANE('',#5979);
#470=PLANE('',#5980);
#471=PLANE('',#5985);
#472=PLANE('',#5986);
#473=PLANE('',#5987);
#474=PLANE('',#5988);
#475=PLANE('',#5989);
#476=PLANE('',#5994);
#477=PLANE('',#5999);
#478=PLANE('',#6009);
#479=PLANE('',#6011);
#480=PLANE('',#6015);
#481=PLANE('',#6027);
#482=PLANE('',#6028);
#483=PLANE('',#6030);
#484=PLANE('',#6031);
#485=PLANE('',#6032);
#486=PLANE('',#6033);
#487=PLANE('',#6034);
#488=PLANE('',#6035);
#489=PLANE('',#6036);
#490=PLANE('',#6037);
#491=PLANE('',#6038);
#492=PLANE('',#6040);
#493=PLANE('',#6048);
#494=PLANE('',#6072);
#495=PLANE('',#6073);
#496=PLANE('',#6075);
#497=PLANE('',#6076);
#498=PLANE('',#6077);
#499=PLANE('',#6082);
#500=PLANE('',#6086);
#501=PLANE('',#6087);
#502=PLANE('',#6088);
#503=PLANE('',#6090);
#504=PLANE('',#6091);
#505=PLANE('',#6092);
#506=PLANE('',#6094);
#507=PLANE('',#6095);
#508=PLANE('',#6097);
#509=PLANE('',#6098);
#510=PLANE('',#6099);
#511=PLANE('',#6104);
#512=PLANE('',#6108);
#513=PLANE('',#6112);
#514=PLANE('',#6113);
#515=PLANE('',#6121);
#516=PLANE('',#6122);
#517=PLANE('',#6130);
#518=PLANE('',#6131);
#519=PLANE('',#6139);
#520=PLANE('',#6140);
#521=PLANE('',#6148);
#522=PLANE('',#6149);
#523=PLANE('',#6157);
#524=PLANE('',#6158);
#525=PLANE('',#6160);
#526=PLANE('',#6165);
#527=PLANE('',#6166);
#528=PLANE('',#6167);
#529=PLANE('',#6168);
#530=PLANE('',#6169);
#531=PLANE('',#6176);
#532=PLANE('',#6178);
#533=PLANE('',#6183);
#534=PLANE('',#6190);
#535=PLANE('',#6191);
#536=PLANE('',#6193);
#537=PLANE('',#6198);
#538=PLANE('',#6205);
#539=PLANE('',#6206);
#540=PLANE('',#6208);
#541=PLANE('',#6209);
#542=PLANE('',#6211);
#543=PLANE('',#6212);
#544=PLANE('',#6224);
#545=PLANE('',#6225);
#546=PLANE('',#6309);
#547=PLANE('',#6310);
#548=PLANE('',#6474);
#549=PLANE('',#6475);
#550=PLANE('',#6476);
#551=PLANE('',#6477);
#552=PLANE('',#6478);
#553=PLANE('',#6479);
#554=PLANE('',#6480);
#555=PLANE('',#6481);
#556=PLANE('',#6482);
#557=PLANE('',#6483);
#558=PLANE('',#6485);
#559=PLANE('',#6493);
#560=PLANE('',#6501);
#561=PLANE('',#6502);
#562=PLANE('',#6503);
#563=PLANE('',#6504);
#564=PLANE('',#6505);
#565=PLANE('',#6506);
#566=PLANE('',#6507);
#567=PLANE('',#6508);
#568=PLANE('',#6509);
#569=PLANE('',#6511);
#570=PLANE('',#6512);
#571=PLANE('',#6513);
#572=PLANE('',#6514);
#573=PLANE('',#6515);
#574=PLANE('',#6516);
#575=PLANE('',#6517);
#576=PLANE('',#6518);
#577=PLANE('',#6519);
#578=PLANE('',#6520);
#579=PLANE('',#6522);
#580=PLANE('',#6523);
#581=PLANE('',#6524);
#582=PLANE('',#6525);
#583=PLANE('',#6526);
#584=PLANE('',#6527);
#585=PLANE('',#6528);
#586=PLANE('',#6529);
#587=PLANE('',#6537);
#588=FACE_OUTER_BOUND('',#902,.T.);
#589=FACE_OUTER_BOUND('',#903,.T.);
#590=FACE_OUTER_BOUND('',#904,.T.);
#591=FACE_OUTER_BOUND('',#905,.T.);
#592=FACE_OUTER_BOUND('',#906,.T.);
#593=FACE_OUTER_BOUND('',#907,.T.);
#594=FACE_OUTER_BOUND('',#908,.T.);
#595=FACE_OUTER_BOUND('',#909,.T.);
#596=FACE_OUTER_BOUND('',#910,.T.);
#597=FACE_OUTER_BOUND('',#915,.T.);
#598=FACE_OUTER_BOUND('',#920,.T.);
#599=FACE_OUTER_BOUND('',#921,.T.);
#600=FACE_OUTER_BOUND('',#922,.T.);
#601=FACE_OUTER_BOUND('',#923,.T.);
#602=FACE_OUTER_BOUND('',#924,.T.);
#603=FACE_OUTER_BOUND('',#925,.T.);
#604=FACE_OUTER_BOUND('',#926,.T.);
#605=FACE_OUTER_BOUND('',#927,.T.);
#606=FACE_OUTER_BOUND('',#928,.T.);
#607=FACE_OUTER_BOUND('',#929,.T.);
#608=FACE_OUTER_BOUND('',#930,.T.);
#609=FACE_OUTER_BOUND('',#931,.T.);
#610=FACE_OUTER_BOUND('',#932,.T.);
#611=FACE_OUTER_BOUND('',#933,.T.);
#612=FACE_OUTER_BOUND('',#934,.T.);
#613=FACE_OUTER_BOUND('',#936,.T.);
#614=FACE_OUTER_BOUND('',#938,.T.);
#615=FACE_OUTER_BOUND('',#939,.T.);
#616=FACE_OUTER_BOUND('',#940,.T.);
#617=FACE_OUTER_BOUND('',#942,.T.);
#618=FACE_OUTER_BOUND('',#944,.T.);
#619=FACE_OUTER_BOUND('',#945,.T.);
#620=FACE_OUTER_BOUND('',#946,.T.);
#621=FACE_OUTER_BOUND('',#948,.T.);
#622=FACE_OUTER_BOUND('',#950,.T.);
#623=FACE_OUTER_BOUND('',#951,.T.);
#624=FACE_OUTER_BOUND('',#952,.T.);
#625=FACE_OUTER_BOUND('',#954,.T.);
#626=FACE_OUTER_BOUND('',#956,.T.);
#627=FACE_OUTER_BOUND('',#957,.T.);
#628=FACE_OUTER_BOUND('',#958,.T.);
#629=FACE_OUTER_BOUND('',#961,.T.);
#630=FACE_OUTER_BOUND('',#962,.T.);
#631=FACE_OUTER_BOUND('',#963,.T.);
#632=FACE_OUTER_BOUND('',#964,.T.);
#633=FACE_OUTER_BOUND('',#965,.T.);
#634=FACE_OUTER_BOUND('',#966,.T.);
#635=FACE_OUTER_BOUND('',#967,.T.);
#636=FACE_OUTER_BOUND('',#971,.T.);
#637=FACE_OUTER_BOUND('',#972,.T.);
#638=FACE_OUTER_BOUND('',#974,.T.);
#639=FACE_OUTER_BOUND('',#976,.T.);
#640=FACE_OUTER_BOUND('',#977,.T.);
#641=FACE_OUTER_BOUND('',#978,.T.);
#642=FACE_OUTER_BOUND('',#979,.T.);
#643=FACE_OUTER_BOUND('',#980,.T.);
#644=FACE_OUTER_BOUND('',#981,.T.);
#645=FACE_OUTER_BOUND('',#982,.T.);
#646=FACE_OUTER_BOUND('',#983,.T.);
#647=FACE_OUTER_BOUND('',#984,.T.);
#648=FACE_OUTER_BOUND('',#985,.T.);
#649=FACE_OUTER_BOUND('',#986,.T.);
#650=FACE_OUTER_BOUND('',#987,.T.);
#651=FACE_OUTER_BOUND('',#991,.T.);
#652=FACE_OUTER_BOUND('',#992,.T.);
#653=FACE_OUTER_BOUND('',#994,.T.);
#654=FACE_OUTER_BOUND('',#997,.T.);
#655=FACE_OUTER_BOUND('',#999,.T.);
#656=FACE_OUTER_BOUND('',#1000,.T.);
#657=FACE_OUTER_BOUND('',#1001,.T.);
#658=FACE_OUTER_BOUND('',#1008,.T.);
#659=FACE_OUTER_BOUND('',#1009,.T.);
#660=FACE_OUTER_BOUND('',#1010,.T.);
#661=FACE_OUTER_BOUND('',#1011,.T.);
#662=FACE_OUTER_BOUND('',#1012,.T.);
#663=FACE_OUTER_BOUND('',#1014,.T.);
#664=FACE_OUTER_BOUND('',#1016,.T.);
#665=FACE_OUTER_BOUND('',#1017,.T.);
#666=FACE_OUTER_BOUND('',#1019,.T.);
#667=FACE_OUTER_BOUND('',#1026,.T.);
#668=FACE_OUTER_BOUND('',#1027,.T.);
#669=FACE_OUTER_BOUND('',#1028,.T.);
#670=FACE_OUTER_BOUND('',#1030,.T.);
#671=FACE_OUTER_BOUND('',#1032,.T.);
#672=FACE_OUTER_BOUND('',#1033,.T.);
#673=FACE_OUTER_BOUND('',#1034,.T.);
#674=FACE_OUTER_BOUND('',#1035,.T.);
#675=FACE_OUTER_BOUND('',#1036,.T.);
#676=FACE_OUTER_BOUND('',#1037,.T.);
#677=FACE_OUTER_BOUND('',#1038,.T.);
#678=FACE_OUTER_BOUND('',#1039,.T.);
#679=FACE_OUTER_BOUND('',#1040,.T.);
#680=FACE_OUTER_BOUND('',#1041,.T.);
#681=FACE_OUTER_BOUND('',#1042,.T.);
#682=FACE_OUTER_BOUND('',#1043,.T.);
#683=FACE_OUTER_BOUND('',#1044,.T.);
#684=FACE_OUTER_BOUND('',#1045,.T.);
#685=FACE_OUTER_BOUND('',#1047,.T.);
#686=FACE_OUTER_BOUND('',#1048,.T.);
#687=FACE_OUTER_BOUND('',#1049,.T.);
#688=FACE_OUTER_BOUND('',#1050,.T.);
#689=FACE_OUTER_BOUND('',#1051,.T.);
#690=FACE_OUTER_BOUND('',#1052,.T.);
#691=FACE_OUTER_BOUND('',#1053,.T.);
#692=FACE_OUTER_BOUND('',#1054,.T.);
#693=FACE_OUTER_BOUND('',#1055,.T.);
#694=FACE_OUTER_BOUND('',#1056,.T.);
#695=FACE_OUTER_BOUND('',#1057,.T.);
#696=FACE_OUTER_BOUND('',#1058,.T.);
#697=FACE_OUTER_BOUND('',#1059,.T.);
#698=FACE_OUTER_BOUND('',#1060,.T.);
#699=FACE_OUTER_BOUND('',#1061,.T.);
#700=FACE_OUTER_BOUND('',#1062,.T.);
#701=FACE_OUTER_BOUND('',#1063,.T.);
#702=FACE_OUTER_BOUND('',#1064,.T.);
#703=FACE_OUTER_BOUND('',#1065,.T.);
#704=FACE_OUTER_BOUND('',#1066,.T.);
#705=FACE_OUTER_BOUND('',#1067,.T.);
#706=FACE_OUTER_BOUND('',#1068,.T.);
#707=FACE_OUTER_BOUND('',#1070,.T.);
#708=FACE_OUTER_BOUND('',#1072,.T.);
#709=FACE_OUTER_BOUND('',#1074,.T.);
#710=FACE_OUTER_BOUND('',#1076,.T.);
#711=FACE_OUTER_BOUND('',#1078,.T.);
#712=FACE_OUTER_BOUND('',#1080,.T.);
#713=FACE_OUTER_BOUND('',#1082,.T.);
#714=FACE_OUTER_BOUND('',#1083,.T.);
#715=FACE_OUTER_BOUND('',#1084,.T.);
#716=FACE_OUTER_BOUND('',#1086,.T.);
#717=FACE_OUTER_BOUND('',#1088,.T.);
#718=FACE_OUTER_BOUND('',#1089,.T.);
#719=FACE_OUTER_BOUND('',#1090,.T.);
#720=FACE_OUTER_BOUND('',#1092,.T.);
#721=FACE_OUTER_BOUND('',#1094,.T.);
#722=FACE_OUTER_BOUND('',#1095,.T.);
#723=FACE_OUTER_BOUND('',#1096,.T.);
#724=FACE_OUTER_BOUND('',#1098,.T.);
#725=FACE_OUTER_BOUND('',#1100,.T.);
#726=FACE_OUTER_BOUND('',#1101,.T.);
#727=FACE_OUTER_BOUND('',#1102,.T.);
#728=FACE_OUTER_BOUND('',#1104,.T.);
#729=FACE_OUTER_BOUND('',#1106,.T.);
#730=FACE_OUTER_BOUND('',#1107,.T.);
#731=FACE_OUTER_BOUND('',#1108,.T.);
#732=FACE_OUTER_BOUND('',#1110,.T.);
#733=FACE_OUTER_BOUND('',#1112,.T.);
#734=FACE_OUTER_BOUND('',#1113,.T.);
#735=FACE_OUTER_BOUND('',#1114,.T.);
#736=FACE_OUTER_BOUND('',#1115,.T.);
#737=FACE_OUTER_BOUND('',#1116,.T.);
#738=FACE_OUTER_BOUND('',#1117,.T.);
#739=FACE_OUTER_BOUND('',#1118,.T.);
#740=FACE_OUTER_BOUND('',#1120,.T.);
#741=FACE_OUTER_BOUND('',#1122,.T.);
#742=FACE_OUTER_BOUND('',#1124,.T.);
#743=FACE_OUTER_BOUND('',#1126,.T.);
#744=FACE_OUTER_BOUND('',#1127,.T.);
#745=FACE_OUTER_BOUND('',#1128,.T.);
#746=FACE_OUTER_BOUND('',#1129,.T.);
#747=FACE_OUTER_BOUND('',#1131,.T.);
#748=FACE_OUTER_BOUND('',#1133,.T.);
#749=FACE_OUTER_BOUND('',#1135,.T.);
#750=FACE_OUTER_BOUND('',#1137,.T.);
#751=FACE_OUTER_BOUND('',#1138,.T.);
#752=FACE_OUTER_BOUND('',#1139,.T.);
#753=FACE_OUTER_BOUND('',#1140,.T.);
#754=FACE_OUTER_BOUND('',#1142,.T.);
#755=FACE_OUTER_BOUND('',#1144,.T.);
#756=FACE_OUTER_BOUND('',#1146,.T.);
#757=FACE_OUTER_BOUND('',#1148,.T.);
#758=FACE_OUTER_BOUND('',#1149,.T.);
#759=FACE_OUTER_BOUND('',#1151,.T.);
#760=FACE_OUTER_BOUND('',#1152,.T.);
#761=FACE_OUTER_BOUND('',#1154,.T.);
#762=FACE_OUTER_BOUND('',#1158,.T.);
#763=FACE_OUTER_BOUND('',#1159,.T.);
#764=FACE_OUTER_BOUND('',#1160,.T.);
#765=FACE_OUTER_BOUND('',#1164,.T.);
#766=FACE_OUTER_BOUND('',#1165,.T.);
#767=FACE_OUTER_BOUND('',#1166,.T.);
#768=FACE_OUTER_BOUND('',#1168,.T.);
#769=FACE_OUTER_BOUND('',#1170,.T.);
#770=FACE_OUTER_BOUND('',#1171,.T.);
#771=FACE_OUTER_BOUND('',#1173,.T.);
#772=FACE_OUTER_BOUND('',#1175,.T.);
#773=FACE_OUTER_BOUND('',#1176,.T.);
#774=FACE_OUTER_BOUND('',#1177,.T.);
#775=FACE_OUTER_BOUND('',#1178,.T.);
#776=FACE_OUTER_BOUND('',#1179,.T.);
#777=FACE_OUTER_BOUND('',#1180,.T.);
#778=FACE_OUTER_BOUND('',#1181,.T.);
#779=FACE_OUTER_BOUND('',#1182,.T.);
#780=FACE_OUTER_BOUND('',#1183,.T.);
#781=FACE_OUTER_BOUND('',#1184,.T.);
#782=FACE_OUTER_BOUND('',#1185,.T.);
#783=FACE_OUTER_BOUND('',#1186,.T.);
#784=FACE_OUTER_BOUND('',#1187,.T.);
#785=FACE_OUTER_BOUND('',#1188,.T.);
#786=FACE_OUTER_BOUND('',#1189,.T.);
#787=FACE_OUTER_BOUND('',#1190,.T.);
#788=FACE_OUTER_BOUND('',#1191,.T.);
#789=FACE_OUTER_BOUND('',#1192,.T.);
#790=FACE_OUTER_BOUND('',#1193,.T.);
#791=FACE_OUTER_BOUND('',#1194,.T.);
#792=FACE_OUTER_BOUND('',#1195,.T.);
#793=FACE_OUTER_BOUND('',#1196,.T.);
#794=FACE_OUTER_BOUND('',#1197,.T.);
#795=FACE_OUTER_BOUND('',#1198,.T.);
#796=FACE_OUTER_BOUND('',#1199,.T.);
#797=FACE_OUTER_BOUND('',#1200,.T.);
#798=FACE_OUTER_BOUND('',#1201,.T.);
#799=FACE_OUTER_BOUND('',#1202,.T.);
#800=FACE_OUTER_BOUND('',#1203,.T.);
#801=FACE_OUTER_BOUND('',#1204,.T.);
#802=FACE_OUTER_BOUND('',#1205,.T.);
#803=FACE_OUTER_BOUND('',#1206,.T.);
#804=FACE_OUTER_BOUND('',#1207,.T.);
#805=FACE_OUTER_BOUND('',#1208,.T.);
#806=FACE_OUTER_BOUND('',#1209,.T.);
#807=FACE_OUTER_BOUND('',#1210,.T.);
#808=FACE_OUTER_BOUND('',#1211,.T.);
#809=FACE_OUTER_BOUND('',#1212,.T.);
#810=FACE_OUTER_BOUND('',#1213,.T.);
#811=FACE_OUTER_BOUND('',#1214,.T.);
#812=FACE_OUTER_BOUND('',#1215,.T.);
#813=FACE_OUTER_BOUND('',#1216,.T.);
#814=FACE_OUTER_BOUND('',#1217,.T.);
#815=FACE_OUTER_BOUND('',#1218,.T.);
#816=FACE_OUTER_BOUND('',#1219,.T.);
#817=FACE_OUTER_BOUND('',#1220,.T.);
#818=FACE_OUTER_BOUND('',#1221,.T.);
#819=FACE_OUTER_BOUND('',#1222,.T.);
#820=FACE_OUTER_BOUND('',#1223,.T.);
#821=FACE_OUTER_BOUND('',#1224,.T.);
#822=FACE_OUTER_BOUND('',#1225,.T.);
#823=FACE_OUTER_BOUND('',#1226,.T.);
#824=FACE_OUTER_BOUND('',#1227,.T.);
#825=FACE_OUTER_BOUND('',#1228,.T.);
#826=FACE_OUTER_BOUND('',#1229,.T.);
#827=FACE_OUTER_BOUND('',#1230,.T.);
#828=FACE_OUTER_BOUND('',#1231,.T.);
#829=FACE_OUTER_BOUND('',#1232,.T.);
#830=FACE_OUTER_BOUND('',#1233,.T.);
#831=FACE_OUTER_BOUND('',#1234,.T.);
#832=FACE_OUTER_BOUND('',#1235,.T.);
#833=FACE_OUTER_BOUND('',#1236,.T.);
#834=FACE_OUTER_BOUND('',#1237,.T.);
#835=FACE_OUTER_BOUND('',#1238,.T.);
#836=FACE_OUTER_BOUND('',#1239,.T.);
#837=FACE_OUTER_BOUND('',#1240,.T.);
#838=FACE_OUTER_BOUND('',#1241,.T.);
#839=FACE_OUTER_BOUND('',#1242,.T.);
#840=FACE_OUTER_BOUND('',#1243,.T.);
#841=FACE_OUTER_BOUND('',#1244,.T.);
#842=FACE_OUTER_BOUND('',#1245,.T.);
#843=FACE_OUTER_BOUND('',#1246,.T.);
#844=FACE_OUTER_BOUND('',#1247,.T.);
#845=FACE_OUTER_BOUND('',#1248,.T.);
#846=FACE_OUTER_BOUND('',#1249,.T.);
#847=FACE_OUTER_BOUND('',#1250,.T.);
#848=FACE_OUTER_BOUND('',#1251,.T.);
#849=FACE_OUTER_BOUND('',#1252,.T.);
#850=FACE_OUTER_BOUND('',#1253,.T.);
#851=FACE_OUTER_BOUND('',#1254,.T.);
#852=FACE_OUTER_BOUND('',#1255,.T.);
#853=FACE_OUTER_BOUND('',#1256,.T.);
#854=FACE_OUTER_BOUND('',#1257,.T.);
#855=FACE_OUTER_BOUND('',#1258,.T.);
#856=FACE_OUTER_BOUND('',#1259,.T.);
#857=FACE_OUTER_BOUND('',#1260,.T.);
#858=FACE_OUTER_BOUND('',#1261,.T.);
#859=FACE_OUTER_BOUND('',#1262,.T.);
#860=FACE_OUTER_BOUND('',#1263,.T.);
#861=FACE_OUTER_BOUND('',#1264,.T.);
#862=FACE_OUTER_BOUND('',#1265,.T.);
#863=FACE_OUTER_BOUND('',#1266,.T.);
#864=FACE_OUTER_BOUND('',#1267,.T.);
#865=FACE_OUTER_BOUND('',#1268,.T.);
#866=FACE_OUTER_BOUND('',#1269,.T.);
#867=FACE_OUTER_BOUND('',#1270,.T.);
#868=FACE_OUTER_BOUND('',#1272,.T.);
#869=FACE_OUTER_BOUND('',#1273,.T.);
#870=FACE_OUTER_BOUND('',#1274,.T.);
#871=FACE_OUTER_BOUND('',#1275,.T.);
#872=FACE_OUTER_BOUND('',#1276,.T.);
#873=FACE_OUTER_BOUND('',#1277,.T.);
#874=FACE_OUTER_BOUND('',#1278,.T.);
#875=FACE_OUTER_BOUND('',#1279,.T.);
#876=FACE_OUTER_BOUND('',#1280,.T.);
#877=FACE_OUTER_BOUND('',#1281,.T.);
#878=FACE_OUTER_BOUND('',#1282,.T.);
#879=FACE_OUTER_BOUND('',#1283,.T.);
#880=FACE_OUTER_BOUND('',#1284,.T.);
#881=FACE_OUTER_BOUND('',#1285,.T.);
#882=FACE_OUTER_BOUND('',#1286,.T.);
#883=FACE_OUTER_BOUND('',#1287,.T.);
#884=FACE_OUTER_BOUND('',#1288,.T.);
#885=FACE_OUTER_BOUND('',#1289,.T.);
#886=FACE_OUTER_BOUND('',#1290,.T.);
#887=FACE_OUTER_BOUND('',#1291,.T.);
#888=FACE_OUTER_BOUND('',#1292,.T.);
#889=FACE_OUTER_BOUND('',#1293,.T.);
#890=FACE_OUTER_BOUND('',#1294,.T.);
#891=FACE_OUTER_BOUND('',#1295,.T.);
#892=FACE_OUTER_BOUND('',#1296,.T.);
#893=FACE_OUTER_BOUND('',#1297,.T.);
#894=FACE_OUTER_BOUND('',#1298,.T.);
#895=FACE_OUTER_BOUND('',#1299,.T.);
#896=FACE_OUTER_BOUND('',#1300,.T.);
#897=FACE_OUTER_BOUND('',#1301,.T.);
#898=FACE_OUTER_BOUND('',#1303,.T.);
#899=FACE_OUTER_BOUND('',#1304,.T.);
#900=FACE_OUTER_BOUND('',#1305,.T.);
#901=FACE_OUTER_BOUND('',#1306,.T.);
#902=EDGE_LOOP('',(#3629,#3630,#3631,#3632));
#903=EDGE_LOOP('',(#3633,#3634,#3635,#3636));
#904=EDGE_LOOP('',(#3637,#3638,#3639,#3640));
#905=EDGE_LOOP('',(#3641,#3642,#3643,#3644));
#906=EDGE_LOOP('',(#3645,#3646,#3647,#3648));
#907=EDGE_LOOP('',(#3649,#3650,#3651,#3652));
#908=EDGE_LOOP('',(#3653,#3654,#3655,#3656));
#909=EDGE_LOOP('',(#3657,#3658,#3659,#3660));
#910=EDGE_LOOP('',(#3661,#3662,#3663,#3664));
#911=EDGE_LOOP('',(#3665));
#912=EDGE_LOOP('',(#3666));
#913=EDGE_LOOP('',(#3667));
#914=EDGE_LOOP('',(#3668));
#915=EDGE_LOOP('',(#3669,#3670,#3671,#3672));
#916=EDGE_LOOP('',(#3673));
#917=EDGE_LOOP('',(#3674));
#918=EDGE_LOOP('',(#3675));
#919=EDGE_LOOP('',(#3676));
#920=EDGE_LOOP('',(#3677,#3678,#3679,#3680));
#921=EDGE_LOOP('',(#3681,#3682,#3683,#3684));
#922=EDGE_LOOP('',(#3685,#3686,#3687,#3688));
#923=EDGE_LOOP('',(#3689,#3690,#3691,#3692));
#924=EDGE_LOOP('',(#3693,#3694,#3695,#3696));
#925=EDGE_LOOP('',(#3697,#3698,#3699,#3700));
#926=EDGE_LOOP('',(#3701,#3702,#3703,#3704));
#927=EDGE_LOOP('',(#3705,#3706,#3707,#3708));
#928=EDGE_LOOP('',(#3709,#3710,#3711,#3712));
#929=EDGE_LOOP('',(#3713,#3714,#3715,#3716));
#930=EDGE_LOOP('',(#3717,#3718,#3719,#3720));
#931=EDGE_LOOP('',(#3721,#3722,#3723,#3724));
#932=EDGE_LOOP('',(#3725,#3726,#3727,#3728));
#933=EDGE_LOOP('',(#3729,#3730,#3731,#3732));
#934=EDGE_LOOP('',(#3733));
#935=EDGE_LOOP('',(#3734));
#936=EDGE_LOOP('',(#3735));
#937=EDGE_LOOP('',(#3736));
#938=EDGE_LOOP('',(#3737,#3738,#3739,#3740));
#939=EDGE_LOOP('',(#3741,#3742,#3743,#3744));
#940=EDGE_LOOP('',(#3745));
#941=EDGE_LOOP('',(#3746));
#942=EDGE_LOOP('',(#3747));
#943=EDGE_LOOP('',(#3748));
#944=EDGE_LOOP('',(#3749,#3750,#3751,#3752));
#945=EDGE_LOOP('',(#3753,#3754,#3755,#3756));
#946=EDGE_LOOP('',(#3757));
#947=EDGE_LOOP('',(#3758));
#948=EDGE_LOOP('',(#3759));
#949=EDGE_LOOP('',(#3760));
#950=EDGE_LOOP('',(#3761,#3762,#3763,#3764));
#951=EDGE_LOOP('',(#3765,#3766,#3767,#3768));
#952=EDGE_LOOP('',(#3769));
#953=EDGE_LOOP('',(#3770));
#954=EDGE_LOOP('',(#3771));
#955=EDGE_LOOP('',(#3772));
#956=EDGE_LOOP('',(#3773,#3774,#3775,#3776));
#957=EDGE_LOOP('',(#3777,#3778,#3779,#3780));
#958=EDGE_LOOP('',(#3781,#3782));
#959=EDGE_LOOP('',(#3783));
#960=EDGE_LOOP('',(#3784));
#961=EDGE_LOOP('',(#3785,#3786,#3787));
#962=EDGE_LOOP('',(#3788,#3789,#3790));
#963=EDGE_LOOP('',(#3791,#3792,#3793));
#964=EDGE_LOOP('',(#3794,#3795,#3796,#3797));
#965=EDGE_LOOP('',(#3798,#3799,#3800));
#966=EDGE_LOOP('',(#3801,#3802,#3803,#3804));
#967=EDGE_LOOP('',(#3805,#3806,#3807,#3808));
#968=EDGE_LOOP('',(#3809));
#969=EDGE_LOOP('',(#3810));
#970=EDGE_LOOP('',(#3811,#3812,#3813,#3814,#3815,#3816,#3817,#3818,#3819,
#3820,#3821,#3822));
#971=EDGE_LOOP('',(#3823,#3824,#3825,#3826,#3827,#3828,#3829,#3830,#3831,
#3832,#3833,#3834));
#972=EDGE_LOOP('',(#3835,#3836));
#973=EDGE_LOOP('',(#3837));
#974=EDGE_LOOP('',(#3838,#3839));
#975=EDGE_LOOP('',(#3840));
#976=EDGE_LOOP('',(#3841,#3842,#3843,#3844));
#977=EDGE_LOOP('',(#3845,#3846,#3847,#3848));
#978=EDGE_LOOP('',(#3849,#3850,#3851,#3852));
#979=EDGE_LOOP('',(#3853,#3854,#3855,#3856));
#980=EDGE_LOOP('',(#3857,#3858,#3859,#3860));
#981=EDGE_LOOP('',(#3861,#3862,#3863,#3864));
#982=EDGE_LOOP('',(#3865,#3866,#3867,#3868));
#983=EDGE_LOOP('',(#3869,#3870,#3871,#3872));
#984=EDGE_LOOP('',(#3873,#3874,#3875,#3876));
#985=EDGE_LOOP('',(#3877,#3878,#3879,#3880));
#986=EDGE_LOOP('',(#3881,#3882,#3883,#3884));
#987=EDGE_LOOP('',(#3885,#3886,#3887,#3888));
#988=EDGE_LOOP('',(#3889,#3890,#3891,#3892));
#989=EDGE_LOOP('',(#3893));
#990=EDGE_LOOP('',(#3894));
#991=EDGE_LOOP('',(#3895,#3896,#3897,#3898));
#992=EDGE_LOOP('',(#3899));
#993=EDGE_LOOP('',(#3900));
#994=EDGE_LOOP('',(#3901,#3902));
#995=EDGE_LOOP('',(#3903));
#996=EDGE_LOOP('',(#3904));
#997=EDGE_LOOP('',(#3905));
#998=EDGE_LOOP('',(#3906));
#999=EDGE_LOOP('',(#3907,#3908,#3909,#3910,#3911,#3912));
#1000=EDGE_LOOP('',(#3913,#3914,#3915,#3916,#3917,#3918));
#1001=EDGE_LOOP('',(#3919,#3920,#3921,#3922));
#1002=EDGE_LOOP('',(#3923,#3924,#3925));
#1003=EDGE_LOOP('',(#3926,#3927,#3928));
#1004=EDGE_LOOP('',(#3929,#3930,#3931));
#1005=EDGE_LOOP('',(#3932,#3933,#3934));
#1006=EDGE_LOOP('',(#3935,#3936,#3937));
#1007=EDGE_LOOP('',(#3938,#3939,#3940));
#1008=EDGE_LOOP('',(#3941,#3942,#3943,#3944,#3945,#3946));
#1009=EDGE_LOOP('',(#3947,#3948,#3949,#3950,#3951,#3952));
#1010=EDGE_LOOP('',(#3953,#3954,#3955,#3956,#3957,#3958));
#1011=EDGE_LOOP('',(#3959,#3960,#3961,#3962,#3963,#3964));
#1012=EDGE_LOOP('',(#3965));
#1013=EDGE_LOOP('',(#3966));
#1014=EDGE_LOOP('',(#3967));
#1015=EDGE_LOOP('',(#3968));
#1016=EDGE_LOOP('',(#3969,#3970,#3971,#3972));
#1017=EDGE_LOOP('',(#3973));
#1018=EDGE_LOOP('',(#3974));
#1019=EDGE_LOOP('',(#3975,#3976,#3977,#3978));
#1020=EDGE_LOOP('',(#3979));
#1021=EDGE_LOOP('',(#3980));
#1022=EDGE_LOOP('',(#3981));
#1023=EDGE_LOOP('',(#3982));
#1024=EDGE_LOOP('',(#3983));
#1025=EDGE_LOOP('',(#3984));
#1026=EDGE_LOOP('',(#3985,#3986,#3987,#3988));
#1027=EDGE_LOOP('',(#3989,#3990,#3991,#3992));
#1028=EDGE_LOOP('',(#3993));
#1029=EDGE_LOOP('',(#3994));
#1030=EDGE_LOOP('',(#3995));
#1031=EDGE_LOOP('',(#3996));
#1032=EDGE_LOOP('',(#3997,#3998,#3999,#4000));
#1033=EDGE_LOOP('',(#4001,#4002,#4003,#4004));
#1034=EDGE_LOOP('',(#4005,#4006,#4007,#4008));
#1035=EDGE_LOOP('',(#4009,#4010,#4011,#4012));
#1036=EDGE_LOOP('',(#4013,#4014,#4015,#4016));
#1037=EDGE_LOOP('',(#4017,#4018,#4019,#4020));
#1038=EDGE_LOOP('',(#4021,#4022,#4023,#4024,#4025,#4026));
#1039=EDGE_LOOP('',(#4027,#4028,#4029,#4030,#4031,#4032));
#1040=EDGE_LOOP('',(#4033));
#1041=EDGE_LOOP('',(#4034));
#1042=EDGE_LOOP('',(#4035,#4036,#4037,#4038));
#1043=EDGE_LOOP('',(#4039,#4040,#4041,#4042));
#1044=EDGE_LOOP('',(#4043,#4044,#4045,#4046));
#1045=EDGE_LOOP('',(#4047));
#1046=EDGE_LOOP('',(#4048));
#1047=EDGE_LOOP('',(#4049,#4050,#4051,#4052));
#1048=EDGE_LOOP('',(#4053,#4054,#4055,#4056));
#1049=EDGE_LOOP('',(#4057,#4058,#4059,#4060));
#1050=EDGE_LOOP('',(#4061,#4062,#4063,#4064));
#1051=EDGE_LOOP('',(#4065,#4066,#4067,#4068));
#1052=EDGE_LOOP('',(#4069,#4070,#4071,#4072));
#1053=EDGE_LOOP('',(#4073,#4074,#4075,#4076));
#1054=EDGE_LOOP('',(#4077,#4078,#4079,#4080));
#1055=EDGE_LOOP('',(#4081));
#1056=EDGE_LOOP('',(#4082,#4083,#4084,#4085));
#1057=EDGE_LOOP('',(#4086));
#1058=EDGE_LOOP('',(#4087,#4088,#4089,#4090));
#1059=EDGE_LOOP('',(#4091,#4092,#4093,#4094));
#1060=EDGE_LOOP('',(#4095,#4096,#4097,#4098));
#1061=EDGE_LOOP('',(#4099,#4100,#4101,#4102));
#1062=EDGE_LOOP('',(#4103,#4104,#4105,#4106));
#1063=EDGE_LOOP('',(#4107,#4108,#4109,#4110));
#1064=EDGE_LOOP('',(#4111,#4112,#4113,#4114));
#1065=EDGE_LOOP('',(#4115,#4116,#4117,#4118));
#1066=EDGE_LOOP('',(#4119,#4120,#4121,#4122));
#1067=EDGE_LOOP('',(#4123,#4124,#4125,#4126));
#1068=EDGE_LOOP('',(#4127,#4128,#4129,#4130));
#1069=EDGE_LOOP('',(#4131,#4132,#4133,#4134));
#1070=EDGE_LOOP('',(#4135));
#1071=EDGE_LOOP('',(#4136));
#1072=EDGE_LOOP('',(#4137,#4138,#4139,#4140));
#1073=EDGE_LOOP('',(#4141,#4142,#4143,#4144));
#1074=EDGE_LOOP('',(#4145));
#1075=EDGE_LOOP('',(#4146));
#1076=EDGE_LOOP('',(#4147,#4148,#4149,#4150));
#1077=EDGE_LOOP('',(#4151,#4152,#4153,#4154));
#1078=EDGE_LOOP('',(#4155));
#1079=EDGE_LOOP('',(#4156));
#1080=EDGE_LOOP('',(#4157));
#1081=EDGE_LOOP('',(#4158));
#1082=EDGE_LOOP('',(#4159,#4160,#4161,#4162));
#1083=EDGE_LOOP('',(#4163,#4164,#4165,#4166));
#1084=EDGE_LOOP('',(#4167));
#1085=EDGE_LOOP('',(#4168));
#1086=EDGE_LOOP('',(#4169));
#1087=EDGE_LOOP('',(#4170));
#1088=EDGE_LOOP('',(#4171,#4172,#4173,#4174));
#1089=EDGE_LOOP('',(#4175,#4176,#4177,#4178));
#1090=EDGE_LOOP('',(#4179));
#1091=EDGE_LOOP('',(#4180));
#1092=EDGE_LOOP('',(#4181));
#1093=EDGE_LOOP('',(#4182));
#1094=EDGE_LOOP('',(#4183,#4184,#4185,#4186));
#1095=EDGE_LOOP('',(#4187,#4188,#4189,#4190));
#1096=EDGE_LOOP('',(#4191));
#1097=EDGE_LOOP('',(#4192));
#1098=EDGE_LOOP('',(#4193));
#1099=EDGE_LOOP('',(#4194));
#1100=EDGE_LOOP('',(#4195,#4196,#4197,#4198));
#1101=EDGE_LOOP('',(#4199,#4200,#4201,#4202));
#1102=EDGE_LOOP('',(#4203));
#1103=EDGE_LOOP('',(#4204));
#1104=EDGE_LOOP('',(#4205));
#1105=EDGE_LOOP('',(#4206));
#1106=EDGE_LOOP('',(#4207,#4208,#4209,#4210));
#1107=EDGE_LOOP('',(#4211,#4212,#4213,#4214));
#1108=EDGE_LOOP('',(#4215));
#1109=EDGE_LOOP('',(#4216));
#1110=EDGE_LOOP('',(#4217));
#1111=EDGE_LOOP('',(#4218));
#1112=EDGE_LOOP('',(#4219,#4220));
#1113=EDGE_LOOP('',(#4221,#4222,#4223,#4224,#4225,#4226,#4227,#4228,#4229));
#1114=EDGE_LOOP('',(#4230,#4231,#4232));
#1115=EDGE_LOOP('',(#4233,#4234,#4235,#4236));
#1116=EDGE_LOOP('',(#4237,#4238,#4239,#4240));
#1117=EDGE_LOOP('',(#4241,#4242,#4243,#4244));
#1118=EDGE_LOOP('',(#4245));
#1119=EDGE_LOOP('',(#4246,#4247,#4248,#4249));
#1120=EDGE_LOOP('',(#4250,#4251,#4252,#4253));
#1121=EDGE_LOOP('',(#4254,#4255,#4256,#4257));
#1122=EDGE_LOOP('',(#4258,#4259,#4260,#4261));
#1123=EDGE_LOOP('',(#4262,#4263));
#1124=EDGE_LOOP('',(#4264));
#1125=EDGE_LOOP('',(#4265,#4266,#4267,#4268));
#1126=EDGE_LOOP('',(#4269,#4270));
#1127=EDGE_LOOP('',(#4271,#4272,#4273,#4274,#4275,#4276,#4277,#4278,#4279));
#1128=EDGE_LOOP('',(#4280,#4281,#4282));
#1129=EDGE_LOOP('',(#4283,#4284,#4285,#4286));
#1130=EDGE_LOOP('',(#4287,#4288,#4289,#4290));
#1131=EDGE_LOOP('',(#4291,#4292,#4293,#4294));
#1132=EDGE_LOOP('',(#4295,#4296));
#1133=EDGE_LOOP('',(#4297));
#1134=EDGE_LOOP('',(#4298));
#1135=EDGE_LOOP('',(#4299));
#1136=EDGE_LOOP('',(#4300));
#1137=EDGE_LOOP('',(#4301,#4302));
#1138=EDGE_LOOP('',(#4303,#4304,#4305,#4306,#4307,#4308,#4309,#4310,#4311));
#1139=EDGE_LOOP('',(#4312,#4313,#4314));
#1140=EDGE_LOOP('',(#4315,#4316,#4317,#4318));
#1141=EDGE_LOOP('',(#4319,#4320,#4321,#4322));
#1142=EDGE_LOOP('',(#4323,#4324,#4325,#4326));
#1143=EDGE_LOOP('',(#4327,#4328));
#1144=EDGE_LOOP('',(#4329));
#1145=EDGE_LOOP('',(#4330));
#1146=EDGE_LOOP('',(#4331));
#1147=EDGE_LOOP('',(#4332));
#1148=EDGE_LOOP('',(#4333,#4334,#4335,#4336));
#1149=EDGE_LOOP('',(#4337,#4338,#4339,#4340));
#1150=EDGE_LOOP('',(#4341));
#1151=EDGE_LOOP('',(#4342,#4343,#4344,#4345));
#1152=EDGE_LOOP('',(#4346));
#1153=EDGE_LOOP('',(#4347,#4348,#4349,#4350));
#1154=EDGE_LOOP('',(#4351,#4352,#4353,#4354));
#1155=EDGE_LOOP('',(#4355,#4356));
#1156=EDGE_LOOP('',(#4357,#4358));
#1157=EDGE_LOOP('',(#4359,#4360));
#1158=EDGE_LOOP('',(#4361,#4362,#4363,#4364,#4365,#4366,#4367));
#1159=EDGE_LOOP('',(#4368,#4369,#4370,#4371,#4372,#4373,#4374));
#1160=EDGE_LOOP('',(#4375,#4376,#4377,#4378,#4379,#4380,#4381,#4382,#4383));
#1161=EDGE_LOOP('',(#4384,#4385,#4386));
#1162=EDGE_LOOP('',(#4387,#4388,#4389));
#1163=EDGE_LOOP('',(#4390,#4391,#4392));
#1164=EDGE_LOOP('',(#4393,#4394,#4395,#4396,#4397,#4398));
#1165=EDGE_LOOP('',(#4399,#4400,#4401,#4402,#4403,#4404,#4405));
#1166=EDGE_LOOP('',(#4406));
#1167=EDGE_LOOP('',(#4407,#4408,#4409,#4410));
#1168=EDGE_LOOP('',(#4411));
#1169=EDGE_LOOP('',(#4412,#4413,#4414,#4415,#4416,#4417,#4418,#4419,#4420,
#4421,#4422,#4423,#4424,#4425,#4426,#4427,#4428,#4429,#4430,#4431,#4432,
#4433,#4434,#4435,#4436,#4437,#4438,#4439,#4440,#4441,#4442,#4443,#4444,
#4445,#4446,#4447,#4448,#4449,#4450,#4451,#4452,#4453,#4454,#4455,#4456,
#4457,#4458,#4459,#4460,#4461,#4462,#4463,#4464,#4465,#4466,#4467,#4468,
#4469,#4470,#4471,#4472,#4473,#4474,#4475,#4476,#4477,#4478,#4479,#4480,
#4481,#4482,#4483,#4484,#4485,#4486,#4487,#4488,#4489,#4490,#4491));
#1170=EDGE_LOOP('',(#4492,#4493,#4494,#4495));
#1171=EDGE_LOOP('',(#4496));
#1172=EDGE_LOOP('',(#4497));
#1173=EDGE_LOOP('',(#4498));
#1174=EDGE_LOOP('',(#4499,#4500,#4501,#4502,#4503,#4504,#4505,#4506,#4507,
#4508,#4509,#4510,#4511,#4512,#4513,#4514,#4515,#4516,#4517,#4518,#4519,
#4520,#4521,#4522,#4523,#4524,#4525,#4526,#4527,#4528,#4529,#4530,#4531,
#4532,#4533,#4534,#4535,#4536,#4537,#4538,#4539,#4540,#4541,#4542,#4543,
#4544,#4545,#4546,#4547,#4548,#4549,#4550,#4551,#4552,#4553,#4554,#4555,
#4556,#4557,#4558,#4559,#4560,#4561,#4562,#4563,#4564,#4565,#4566,#4567,
#4568,#4569,#4570,#4571,#4572,#4573,#4574,#4575,#4576,#4577,#4578));
#1175=EDGE_LOOP('',(#4579,#4580,#4581,#4582));
#1176=EDGE_LOOP('',(#4583,#4584,#4585,#4586));
#1177=EDGE_LOOP('',(#4587,#4588,#4589,#4590));
#1178=EDGE_LOOP('',(#4591,#4592,#4593,#4594));
#1179=EDGE_LOOP('',(#4595,#4596,#4597,#4598));
#1180=EDGE_LOOP('',(#4599,#4600,#4601,#4602));
#1181=EDGE_LOOP('',(#4603,#4604,#4605,#4606));
#1182=EDGE_LOOP('',(#4607,#4608,#4609,#4610));
#1183=EDGE_LOOP('',(#4611,#4612,#4613,#4614));
#1184=EDGE_LOOP('',(#4615,#4616,#4617,#4618));
#1185=EDGE_LOOP('',(#4619,#4620,#4621,#4622));
#1186=EDGE_LOOP('',(#4623,#4624,#4625,#4626));
#1187=EDGE_LOOP('',(#4627,#4628,#4629,#4630));
#1188=EDGE_LOOP('',(#4631,#4632,#4633,#4634));
#1189=EDGE_LOOP('',(#4635,#4636,#4637,#4638));
#1190=EDGE_LOOP('',(#4639,#4640,#4641,#4642));
#1191=EDGE_LOOP('',(#4643,#4644,#4645,#4646));
#1192=EDGE_LOOP('',(#4647,#4648,#4649,#4650));
#1193=EDGE_LOOP('',(#4651,#4652,#4653,#4654));
#1194=EDGE_LOOP('',(#4655,#4656,#4657,#4658));
#1195=EDGE_LOOP('',(#4659,#4660,#4661,#4662));
#1196=EDGE_LOOP('',(#4663,#4664,#4665,#4666));
#1197=EDGE_LOOP('',(#4667,#4668,#4669,#4670));
#1198=EDGE_LOOP('',(#4671,#4672,#4673,#4674));
#1199=EDGE_LOOP('',(#4675,#4676,#4677,#4678));
#1200=EDGE_LOOP('',(#4679,#4680,#4681,#4682));
#1201=EDGE_LOOP('',(#4683,#4684,#4685,#4686));
#1202=EDGE_LOOP('',(#4687,#4688,#4689,#4690));
#1203=EDGE_LOOP('',(#4691,#4692,#4693,#4694));
#1204=EDGE_LOOP('',(#4695,#4696,#4697,#4698));
#1205=EDGE_LOOP('',(#4699,#4700,#4701,#4702));
#1206=EDGE_LOOP('',(#4703,#4704,#4705,#4706));
#1207=EDGE_LOOP('',(#4707,#4708,#4709,#4710));
#1208=EDGE_LOOP('',(#4711,#4712,#4713,#4714));
#1209=EDGE_LOOP('',(#4715,#4716,#4717,#4718));
#1210=EDGE_LOOP('',(#4719,#4720,#4721,#4722));
#1211=EDGE_LOOP('',(#4723,#4724,#4725,#4726));
#1212=EDGE_LOOP('',(#4727,#4728,#4729,#4730));
#1213=EDGE_LOOP('',(#4731,#4732,#4733,#4734));
#1214=EDGE_LOOP('',(#4735,#4736,#4737,#4738));
#1215=EDGE_LOOP('',(#4739,#4740,#4741,#4742));
#1216=EDGE_LOOP('',(#4743,#4744,#4745,#4746));
#1217=EDGE_LOOP('',(#4747,#4748,#4749,#4750));
#1218=EDGE_LOOP('',(#4751,#4752,#4753,#4754));
#1219=EDGE_LOOP('',(#4755,#4756,#4757,#4758));
#1220=EDGE_LOOP('',(#4759,#4760,#4761,#4762));
#1221=EDGE_LOOP('',(#4763,#4764,#4765,#4766));
#1222=EDGE_LOOP('',(#4767,#4768,#4769,#4770));
#1223=EDGE_LOOP('',(#4771,#4772,#4773,#4774));
#1224=EDGE_LOOP('',(#4775,#4776,#4777,#4778));
#1225=EDGE_LOOP('',(#4779,#4780,#4781,#4782));
#1226=EDGE_LOOP('',(#4783,#4784,#4785,#4786));
#1227=EDGE_LOOP('',(#4787,#4788,#4789,#4790));
#1228=EDGE_LOOP('',(#4791,#4792,#4793,#4794));
#1229=EDGE_LOOP('',(#4795,#4796,#4797,#4798));
#1230=EDGE_LOOP('',(#4799,#4800,#4801,#4802));
#1231=EDGE_LOOP('',(#4803,#4804,#4805,#4806));
#1232=EDGE_LOOP('',(#4807,#4808,#4809,#4810));
#1233=EDGE_LOOP('',(#4811,#4812,#4813,#4814));
#1234=EDGE_LOOP('',(#4815,#4816,#4817,#4818));
#1235=EDGE_LOOP('',(#4819,#4820,#4821,#4822));
#1236=EDGE_LOOP('',(#4823,#4824,#4825,#4826));
#1237=EDGE_LOOP('',(#4827,#4828,#4829,#4830));
#1238=EDGE_LOOP('',(#4831,#4832,#4833,#4834));
#1239=EDGE_LOOP('',(#4835,#4836,#4837,#4838));
#1240=EDGE_LOOP('',(#4839,#4840,#4841,#4842));
#1241=EDGE_LOOP('',(#4843,#4844,#4845,#4846));
#1242=EDGE_LOOP('',(#4847,#4848,#4849,#4850));
#1243=EDGE_LOOP('',(#4851,#4852,#4853,#4854));
#1244=EDGE_LOOP('',(#4855,#4856,#4857,#4858));
#1245=EDGE_LOOP('',(#4859,#4860,#4861,#4862));
#1246=EDGE_LOOP('',(#4863,#4864,#4865,#4866));
#1247=EDGE_LOOP('',(#4867,#4868,#4869,#4870));
#1248=EDGE_LOOP('',(#4871,#4872,#4873,#4874));
#1249=EDGE_LOOP('',(#4875,#4876,#4877,#4878));
#1250=EDGE_LOOP('',(#4879,#4880,#4881,#4882));
#1251=EDGE_LOOP('',(#4883,#4884,#4885,#4886));
#1252=EDGE_LOOP('',(#4887,#4888,#4889,#4890));
#1253=EDGE_LOOP('',(#4891,#4892,#4893,#4894));
#1254=EDGE_LOOP('',(#4895,#4896,#4897,#4898));
#1255=EDGE_LOOP('',(#4899,#4900,#4901,#4902));
#1256=EDGE_LOOP('',(#4903,#4904,#4905,#4906,#4907,#4908,#4909,#4910));
#1257=EDGE_LOOP('',(#4911,#4912,#4913,#4914));
#1258=EDGE_LOOP('',(#4915,#4916,#4917,#4918));
#1259=EDGE_LOOP('',(#4919,#4920,#4921,#4922));
#1260=EDGE_LOOP('',(#4923,#4924,#4925,#4926));
#1261=EDGE_LOOP('',(#4927,#4928,#4929,#4930,#4931,#4932,#4933,#4934));
#1262=EDGE_LOOP('',(#4935,#4936,#4937,#4938));
#1263=EDGE_LOOP('',(#4939,#4940,#4941,#4942));
#1264=EDGE_LOOP('',(#4943,#4944,#4945,#4946));
#1265=EDGE_LOOP('',(#4947,#4948,#4949,#4950));
#1266=EDGE_LOOP('',(#4951));
#1267=EDGE_LOOP('',(#4952,#4953,#4954,#4955));
#1268=EDGE_LOOP('',(#4956,#4957,#4958,#4959));
#1269=EDGE_LOOP('',(#4960,#4961,#4962,#4963));
#1270=EDGE_LOOP('',(#4964));
#1271=EDGE_LOOP('',(#4965));
#1272=EDGE_LOOP('',(#4966,#4967,#4968,#4969));
#1273=EDGE_LOOP('',(#4970,#4971,#4972,#4973));
#1274=EDGE_LOOP('',(#4974,#4975,#4976,#4977));
#1275=EDGE_LOOP('',(#4978));
#1276=EDGE_LOOP('',(#4979,#4980,#4981,#4982));
#1277=EDGE_LOOP('',(#4983,#4984,#4985,#4986));
#1278=EDGE_LOOP('',(#4987,#4988,#4989,#4990));
#1279=EDGE_LOOP('',(#4991,#4992,#4993,#4994));
#1280=EDGE_LOOP('',(#4995,#4996,#4997,#4998));
#1281=EDGE_LOOP('',(#4999,#5000,#5001,#5002));
#1282=EDGE_LOOP('',(#5003,#5004,#5005,#5006,#5007,#5008));
#1283=EDGE_LOOP('',(#5009,#5010,#5011,#5012,#5013,#5014));
#1284=EDGE_LOOP('',(#5015,#5016,#5017,#5018,#5019,#5020,#5021,#5022));
#1285=EDGE_LOOP('',(#5023,#5024,#5025,#5026));
#1286=EDGE_LOOP('',(#5027,#5028,#5029,#5030));
#1287=EDGE_LOOP('',(#5031,#5032,#5033,#5034));
#1288=EDGE_LOOP('',(#5035,#5036,#5037,#5038));
#1289=EDGE_LOOP('',(#5039,#5040,#5041,#5042,#5043,#5044,#5045,#5046));
#1290=EDGE_LOOP('',(#5047,#5048,#5049,#5050));
#1291=EDGE_LOOP('',(#5051,#5052,#5053,#5054));
#1292=EDGE_LOOP('',(#5055,#5056,#5057,#5058));
#1293=EDGE_LOOP('',(#5059,#5060,#5061,#5062));
#1294=EDGE_LOOP('',(#5063,#5064,#5065,#5066));
#1295=EDGE_LOOP('',(#5067,#5068,#5069,#5070));
#1296=EDGE_LOOP('',(#5071,#5072,#5073,#5074));
#1297=EDGE_LOOP('',(#5075,#5076,#5077,#5078));
#1298=EDGE_LOOP('',(#5079,#5080,#5081,#5082));
#1299=EDGE_LOOP('',(#5083,#5084,#5085,#5086));
#1300=EDGE_LOOP('',(#5087,#5088,#5089,#5090,#5091,#5092));
#1301=EDGE_LOOP('',(#5093));
#1302=EDGE_LOOP('',(#5094,#5095,#5096,#5097,#5098,#5099));
#1303=EDGE_LOOP('',(#5100,#5101,#5102,#5103));
#1304=EDGE_LOOP('',(#5104,#5105,#5106,#5107));
#1305=EDGE_LOOP('',(#5108,#5109,#5110,#5111));
#1306=EDGE_LOOP('',(#5112));
#1307=LINE('',#8319,#1696);
#1308=LINE('',#8325,#1697);
#1309=LINE('',#8331,#1698);
#1310=LINE('',#8337,#1699);
#1311=LINE('',#8342,#1700);
#1312=LINE('',#8344,#1701);
#1313=LINE('',#8346,#1702);
#1314=LINE('',#8347,#1703);
#1315=LINE('',#8350,#1704);
#1316=LINE('',#8352,#1705);
#1317=LINE('',#8353,#1706);
#1318=LINE('',#8356,#1707);
#1319=LINE('',#8358,#1708);
#1320=LINE('',#8359,#1709);
#1321=LINE('',#8361,#1710);
#1322=LINE('',#8362,#1711);
#1323=LINE('',#8369,#1712);
#1324=LINE('',#8371,#1713);
#1325=LINE('',#8373,#1714);
#1326=LINE('',#8374,#1715);
#1327=LINE('',#8377,#1716);
#1328=LINE('',#8379,#1717);
#1329=LINE('',#8380,#1718);
#1330=LINE('',#8383,#1719);
#1331=LINE('',#8385,#1720);
#1332=LINE('',#8386,#1721);
#1333=LINE('',#8388,#1722);
#1334=LINE('',#8389,#1723);
#1335=LINE('',#8396,#1724);
#1336=LINE('',#8398,#1725);
#1337=LINE('',#8400,#1726);
#1338=LINE('',#8401,#1727);
#1339=LINE('',#8404,#1728);
#1340=LINE('',#8406,#1729);
#1341=LINE('',#8407,#1730);
#1342=LINE('',#8410,#1731);
#1343=LINE('',#8412,#1732);
#1344=LINE('',#8413,#1733);
#1345=LINE('',#8415,#1734);
#1346=LINE('',#8416,#1735);
#1347=LINE('',#8424,#1736);
#1348=LINE('',#8430,#1737);
#1349=LINE('',#8439,#1738);
#1350=LINE('',#8445,#1739);
#1351=LINE('',#8454,#1740);
#1352=LINE('',#8460,#1741);
#1353=LINE('',#8469,#1742);
#1354=LINE('',#8475,#1743);
#1355=LINE('',#8485,#1744);
#1356=LINE('',#8491,#1745);
#1357=LINE('',#8500,#1746);
#1358=LINE('',#8502,#1747);
#1359=LINE('',#8507,#1748);
#1360=LINE('',#8510,#1749);
#1361=LINE('',#8514,#1750);
#1362=LINE('',#8517,#1751);
#1363=LINE('',#8519,#1752);
#1364=LINE('',#8520,#1753);
#1365=LINE('',#8524,#1754);
#1366=LINE('',#8526,#1755);
#1367=LINE('',#8529,#1756);
#1368=LINE('',#8530,#1757);
#1369=LINE('',#8534,#1758);
#1370=LINE('',#8536,#1759);
#1371=LINE('',#8538,#1760);
#1372=LINE('',#8539,#1761);
#1373=LINE('',#8545,#1762);
#1374=LINE('',#8547,#1763);
#1375=LINE('',#8548,#1764);
#1376=LINE('',#8550,#1765);
#1377=LINE('',#8552,#1766);
#1378=LINE('',#8553,#1767);
#1379=LINE('',#8562,#1768);
#1380=LINE('',#8564,#1769);
#1381=LINE('',#8566,#1770);
#1382=LINE('',#8567,#1771);
#1383=LINE('',#8570,#1772);
#1384=LINE('',#8572,#1773);
#1385=LINE('',#8573,#1774);
#1386=LINE('',#8576,#1775);
#1387=LINE('',#8578,#1776);
#1388=LINE('',#8579,#1777);
#1389=LINE('',#8581,#1778);
#1390=LINE('',#8582,#1779);
#1391=LINE('',#8587,#1780);
#1392=LINE('',#8591,#1781);
#1393=LINE('',#8595,#1782);
#1394=LINE('',#8596,#1783);
#1395=LINE('',#8597,#1784);
#1396=LINE('',#8600,#1785);
#1397=LINE('',#8601,#1786);
#1398=LINE('',#8604,#1787);
#1399=LINE('',#8605,#1788);
#1400=LINE('',#8607,#1789);
#1401=LINE('',#8614,#1790);
#1402=LINE('',#8669,#1791);
#1403=LINE('',#8741,#1792);
#1404=LINE('',#8786,#1793);
#1405=LINE('',#8954,#1794);
#1406=LINE('',#9025,#1795);
#1407=LINE('',#9028,#1796);
#1408=LINE('',#9099,#1797);
#1409=LINE('',#9109,#1798);
#1410=LINE('',#9114,#1799);
#1411=LINE('',#9122,#1800);
#1412=LINE('',#9128,#1801);
#1413=LINE('',#9136,#1802);
#1414=LINE('',#9138,#1803);
#1415=LINE('',#9140,#1804);
#1416=LINE('',#9141,#1805);
#1417=LINE('',#9144,#1806);
#1418=LINE('',#9146,#1807);
#1419=LINE('',#9147,#1808);
#1420=LINE('',#9150,#1809);
#1421=LINE('',#9152,#1810);
#1422=LINE('',#9153,#1811);
#1423=LINE('',#9156,#1812);
#1424=LINE('',#9158,#1813);
#1425=LINE('',#9159,#1814);
#1426=LINE('',#9162,#1815);
#1427=LINE('',#9164,#1816);
#1428=LINE('',#9165,#1817);
#1429=LINE('',#9167,#1818);
#1430=LINE('',#9168,#1819);
#1431=LINE('',#9180,#1820);
#1432=LINE('',#9184,#1821);
#1433=LINE('',#9188,#1822);
#1434=LINE('',#9195,#1823);
#1435=LINE('',#9197,#1824);
#1436=LINE('',#9220,#1825);
#1437=LINE('',#9222,#1826);
#1438=LINE('',#9224,#1827);
#1439=LINE('',#9225,#1828);
#1440=LINE('',#9230,#1829);
#1441=LINE('',#9231,#1830);
#1442=LINE('',#9234,#1831);
#1443=LINE('',#9236,#1832);
#1444=LINE('',#9237,#1833);
#1445=LINE('',#9239,#1834);
#1446=LINE('',#9246,#1835);
#1447=LINE('',#9253,#1836);
#1448=LINE('',#9259,#1837);
#1449=LINE('',#9261,#1838);
#1450=LINE('',#9263,#1839);
#1451=LINE('',#9264,#1840);
#1452=LINE('',#9269,#1841);
#1453=LINE('',#9270,#1842);
#1454=LINE('',#9273,#1843);
#1455=LINE('',#9275,#1844);
#1456=LINE('',#9276,#1845);
#1457=LINE('',#9278,#1846);
#1458=LINE('',#9284,#1847);
#1459=LINE('',#9286,#1848);
#1460=LINE('',#9288,#1849);
#1461=LINE('',#9289,#1850);
#1462=LINE('',#9294,#1851);
#1463=LINE('',#9295,#1852);
#1464=LINE('',#9298,#1853);
#1465=LINE('',#9300,#1854);
#1466=LINE('',#9301,#1855);
#1467=LINE('',#9303,#1856);
#1468=LINE('',#9310,#1857);
#1469=LINE('',#9317,#1858);
#1470=LINE('',#9324,#1859);
#1471=LINE('',#9333,#1860);
#1472=LINE('',#9339,#1861);
#1473=LINE('',#9348,#1862);
#1474=LINE('',#9354,#1863);
#1475=LINE('',#9363,#1864);
#1476=LINE('',#9369,#1865);
#1477=LINE('',#9378,#1866);
#1478=LINE('',#9384,#1867);
#1479=LINE('',#9393,#1868);
#1480=LINE('',#9399,#1869);
#1481=LINE('',#9407,#1870);
#1482=LINE('',#9424,#1871);
#1483=LINE('',#9475,#1872);
#1484=LINE('',#9479,#1873);
#1485=LINE('',#9481,#1874);
#1486=LINE('',#9483,#1875);
#1487=LINE('',#9484,#1876);
#1488=LINE('',#9487,#1877);
#1489=LINE('',#9489,#1878);
#1490=LINE('',#9490,#1879);
#1491=LINE('',#9493,#1880);
#1492=LINE('',#9495,#1881);
#1493=LINE('',#9496,#1882);
#1494=LINE('',#9505,#1883);
#1495=LINE('',#9512,#1884);
#1496=LINE('',#9533,#1885);
#1497=LINE('',#9588,#1886);
#1498=LINE('',#9593,#1887);
#1499=LINE('',#9599,#1888);
#1500=LINE('',#9607,#1889);
#1501=LINE('',#9628,#1890);
#1502=LINE('',#9683,#1891);
#1503=LINE('',#9688,#1892);
#1504=LINE('',#9694,#1893);
#1505=LINE('',#9702,#1894);
#1506=LINE('',#9704,#1895);
#1507=LINE('',#9706,#1896);
#1508=LINE('',#9707,#1897);
#1509=LINE('',#9710,#1898);
#1510=LINE('',#9712,#1899);
#1511=LINE('',#9713,#1900);
#1512=LINE('',#9718,#1901);
#1513=LINE('',#9720,#1902);
#1514=LINE('',#9721,#1903);
#1515=LINE('',#9884,#1904);
#1516=LINE('',#9887,#1905);
#1517=LINE('',#9931,#1906);
#1518=LINE('',#9933,#1907);
#1519=LINE('',#10018,#1908);
#1520=LINE('',#10020,#1909);
#1521=LINE('',#10188,#1910);
#1522=LINE('',#10354,#1911);
#1523=LINE('',#10356,#1912);
#1524=LINE('',#10357,#1913);
#1525=LINE('',#10359,#1914);
#1526=LINE('',#10361,#1915);
#1527=LINE('',#10363,#1916);
#1528=LINE('',#10365,#1917);
#1529=LINE('',#10367,#1918);
#1530=LINE('',#10369,#1919);
#1531=LINE('',#10371,#1920);
#1532=LINE('',#10373,#1921);
#1533=LINE('',#10375,#1922);
#1534=LINE('',#10377,#1923);
#1535=LINE('',#10379,#1924);
#1536=LINE('',#10381,#1925);
#1537=LINE('',#10383,#1926);
#1538=LINE('',#10385,#1927);
#1539=LINE('',#10387,#1928);
#1540=LINE('',#10389,#1929);
#1541=LINE('',#10391,#1930);
#1542=LINE('',#10393,#1931);
#1543=LINE('',#10395,#1932);
#1544=LINE('',#10397,#1933);
#1545=LINE('',#10399,#1934);
#1546=LINE('',#10401,#1935);
#1547=LINE('',#10403,#1936);
#1548=LINE('',#10405,#1937);
#1549=LINE('',#10407,#1938);
#1550=LINE('',#10409,#1939);
#1551=LINE('',#10411,#1940);
#1552=LINE('',#10413,#1941);
#1553=LINE('',#10415,#1942);
#1554=LINE('',#10417,#1943);
#1555=LINE('',#10419,#1944);
#1556=LINE('',#10421,#1945);
#1557=LINE('',#10423,#1946);
#1558=LINE('',#10425,#1947);
#1559=LINE('',#10427,#1948);
#1560=LINE('',#10429,#1949);
#1561=LINE('',#10431,#1950);
#1562=LINE('',#10433,#1951);
#1563=LINE('',#10435,#1952);
#1564=LINE('',#10437,#1953);
#1565=LINE('',#10439,#1954);
#1566=LINE('',#10441,#1955);
#1567=LINE('',#10443,#1956);
#1568=LINE('',#10445,#1957);
#1569=LINE('',#10447,#1958);
#1570=LINE('',#10449,#1959);
#1571=LINE('',#10451,#1960);
#1572=LINE('',#10453,#1961);
#1573=LINE('',#10455,#1962);
#1574=LINE('',#10457,#1963);
#1575=LINE('',#10459,#1964);
#1576=LINE('',#10461,#1965);
#1577=LINE('',#10463,#1966);
#1578=LINE('',#10465,#1967);
#1579=LINE('',#10467,#1968);
#1580=LINE('',#10469,#1969);
#1581=LINE('',#10471,#1970);
#1582=LINE('',#10473,#1971);
#1583=LINE('',#10475,#1972);
#1584=LINE('',#10477,#1973);
#1585=LINE('',#10479,#1974);
#1586=LINE('',#10481,#1975);
#1587=LINE('',#10483,#1976);
#1588=LINE('',#10485,#1977);
#1589=LINE('',#10487,#1978);
#1590=LINE('',#10489,#1979);
#1591=LINE('',#10491,#1980);
#1592=LINE('',#10493,#1981);
#1593=LINE('',#10495,#1982);
#1594=LINE('',#10497,#1983);
#1595=LINE('',#10499,#1984);
#1596=LINE('',#10501,#1985);
#1597=LINE('',#10503,#1986);
#1598=LINE('',#10505,#1987);
#1599=LINE('',#10507,#1988);
#1600=LINE('',#10509,#1989);
#1601=LINE('',#10511,#1990);
#1602=LINE('',#10513,#1991);
#1603=LINE('',#10519,#1992);
#1604=LINE('',#10521,#1993);
#1605=LINE('',#10523,#1994);
#1606=LINE('',#10525,#1995);
#1607=LINE('',#10527,#1996);
#1608=LINE('',#10529,#1997);
#1609=LINE('',#10531,#1998);
#1610=LINE('',#10532,#1999);
#1611=LINE('',#10535,#2000);
#1612=LINE('',#10537,#2001);
#1613=LINE('',#10538,#2002);
#1614=LINE('',#10541,#2003);
#1615=LINE('',#10542,#2004);
#1616=LINE('',#10545,#2005);
#1617=LINE('',#10546,#2006);
#1618=LINE('',#10549,#2007);
#1619=LINE('',#10550,#2008);
#1620=LINE('',#10553,#2009);
#1621=LINE('',#10555,#2010);
#1622=LINE('',#10557,#2011);
#1623=LINE('',#10558,#2012);
#1624=LINE('',#10560,#2013);
#1625=LINE('',#10562,#2014);
#1626=LINE('',#10564,#2015);
#1627=LINE('',#10573,#2016);
#1628=LINE('',#10577,#2017);
#1629=LINE('',#10581,#2018);
#1630=LINE('',#10588,#2019);
#1631=LINE('',#10592,#2020);
#1632=LINE('',#10596,#2021);
#1633=LINE('',#10601,#2022);
#1634=LINE('',#10603,#2023);
#1635=LINE('',#10605,#2024);
#1636=LINE('',#10606,#2025);
#1637=LINE('',#10609,#2026);
#1638=LINE('',#10611,#2027);
#1639=LINE('',#10612,#2028);
#1640=LINE('',#10615,#2029);
#1641=LINE('',#10617,#2030);
#1642=LINE('',#10618,#2031);
#1643=LINE('',#10621,#2032);
#1644=LINE('',#10623,#2033);
#1645=LINE('',#10624,#2034);
#1646=LINE('',#10627,#2035);
#1647=LINE('',#10629,#2036);
#1648=LINE('',#10630,#2037);
#1649=LINE('',#10632,#2038);
#1650=LINE('',#10633,#2039);
#1651=LINE('',#10640,#2040);
#1652=LINE('',#10642,#2041);
#1653=LINE('',#10644,#2042);
#1654=LINE('',#10646,#2043);
#1655=LINE('',#10648,#2044);
#1656=LINE('',#10650,#2045);
#1657=LINE('',#10652,#2046);
#1658=LINE('',#10653,#2047);
#1659=LINE('',#10656,#2048);
#1660=LINE('',#10658,#2049);
#1661=LINE('',#10659,#2050);
#1662=LINE('',#10662,#2051);
#1663=LINE('',#10663,#2052);
#1664=LINE('',#10666,#2053);
#1665=LINE('',#10667,#2054);
#1666=LINE('',#10670,#2055);
#1667=LINE('',#10671,#2056);
#1668=LINE('',#10675,#2057);
#1669=LINE('',#10676,#2058);
#1670=LINE('',#10678,#2059);
#1671=LINE('',#10679,#2060);
#1672=LINE('',#10681,#2061);
#1673=LINE('',#10683,#2062);
#1674=LINE('',#10685,#2063);
#1675=LINE('',#10691,#2064);
#1676=LINE('',#10693,#2065);
#1677=LINE('',#10695,#2066);
#1678=LINE('',#10696,#2067);
#1679=LINE('',#10699,#2068);
#1680=LINE('',#10701,#2069);
#1681=LINE('',#10702,#2070);
#1682=LINE('',#10705,#2071);
#1683=LINE('',#10707,#2072);
#1684=LINE('',#10708,#2073);
#1685=LINE('',#10711,#2074);
#1686=LINE('',#10713,#2075);
#1687=LINE('',#10714,#2076);
#1688=LINE('',#10717,#2077);
#1689=LINE('',#10719,#2078);
#1690=LINE('',#10720,#2079);
#1691=LINE('',#10722,#2080);
#1692=LINE('',#10723,#2081);
#1693=LINE('',#10731,#2082);
#1694=LINE('',#10735,#2083);
#1695=LINE('',#10739,#2084);
#1696=VECTOR('',#6569,0.34);
#1697=VECTOR('',#6576,0.34);
#1698=VECTOR('',#6583,0.34);
#1699=VECTOR('',#6590,0.34);
#1700=VECTOR('',#6595,1.);
#1701=VECTOR('',#6596,1.);
#1702=VECTOR('',#6597,1.);
#1703=VECTOR('',#6598,1.);
#1704=VECTOR('',#6601,1.);
#1705=VECTOR('',#6602,1.);
#1706=VECTOR('',#6603,1.);
#1707=VECTOR('',#6606,1.);
#1708=VECTOR('',#6607,1.);
#1709=VECTOR('',#6608,1.);
#1710=VECTOR('',#6611,1.);
#1711=VECTOR('',#6612,1.);
#1712=VECTOR('',#6621,1.);
#1713=VECTOR('',#6622,1.);
#1714=VECTOR('',#6623,1.);
#1715=VECTOR('',#6624,1.);
#1716=VECTOR('',#6627,1.);
#1717=VECTOR('',#6628,1.);
#1718=VECTOR('',#6629,1.);
#1719=VECTOR('',#6632,1.);
#1720=VECTOR('',#6633,1.);
#1721=VECTOR('',#6634,1.);
#1722=VECTOR('',#6637,1.);
#1723=VECTOR('',#6638,1.);
#1724=VECTOR('',#6647,1.);
#1725=VECTOR('',#6648,1.);
#1726=VECTOR('',#6649,1.);
#1727=VECTOR('',#6650,1.);
#1728=VECTOR('',#6653,1.);
#1729=VECTOR('',#6654,1.);
#1730=VECTOR('',#6655,1.);
#1731=VECTOR('',#6658,1.);
#1732=VECTOR('',#6659,1.);
#1733=VECTOR('',#6660,1.);
#1734=VECTOR('',#6663,1.);
#1735=VECTOR('',#6664,1.);
#1736=VECTOR('',#6675,0.425);
#1737=VECTOR('',#6682,0.645);
#1738=VECTOR('',#6695,0.425);
#1739=VECTOR('',#6702,0.645);
#1740=VECTOR('',#6715,0.425);
#1741=VECTOR('',#6722,0.645);
#1742=VECTOR('',#6735,0.425);
#1743=VECTOR('',#6742,0.645);
#1744=VECTOR('',#6757,2.05);
#1745=VECTOR('',#6764,2.05);
#1746=VECTOR('',#6773,1.);
#1747=VECTOR('',#6774,1.);
#1748=VECTOR('',#6779,1.);
#1749=VECTOR('',#6782,1.);
#1750=VECTOR('',#6785,1.);
#1751=VECTOR('',#6788,1.);
#1752=VECTOR('',#6791,1.);
#1753=VECTOR('',#6792,1.);
#1754=VECTOR('',#6795,1.);
#1755=VECTOR('',#6796,1.);
#1756=VECTOR('',#6801,1.);
#1757=VECTOR('',#6802,1.);
#1758=VECTOR('',#6805,1.);
#1759=VECTOR('',#6806,1.);
#1760=VECTOR('',#6807,1.);
#1761=VECTOR('',#6808,1.);
#1762=VECTOR('',#6813,1.);
#1763=VECTOR('',#6814,1.);
#1764=VECTOR('',#6815,1.);
#1765=VECTOR('',#6816,1.);
#1766=VECTOR('',#6817,1.);
#1767=VECTOR('',#6818,1.);
#1768=VECTOR('',#6831,1.);
#1769=VECTOR('',#6832,1.);
#1770=VECTOR('',#6833,1.);
#1771=VECTOR('',#6834,1.);
#1772=VECTOR('',#6837,1.);
#1773=VECTOR('',#6838,1.);
#1774=VECTOR('',#6839,1.);
#1775=VECTOR('',#6842,1.);
#1776=VECTOR('',#6843,1.);
#1777=VECTOR('',#6844,1.);
#1778=VECTOR('',#6847,1.);
#1779=VECTOR('',#6848,1.);
#1780=VECTOR('',#6855,0.65);
#1781=VECTOR('',#6860,0.65);
#1782=VECTOR('',#6863,1.);
#1783=VECTOR('',#6864,1.);
#1784=VECTOR('',#6865,1.);
#1785=VECTOR('',#6868,1.);
#1786=VECTOR('',#6869,1.);
#1787=VECTOR('',#6872,1.);
#1788=VECTOR('',#6873,1.);
#1789=VECTOR('',#6876,1.);
#1790=VECTOR('',#6885,1.8);
#1791=VECTOR('',#6902,0.25);
#1792=VECTOR('',#6905,0.25);
#1793=VECTOR('',#6910,1.65);
#1794=VECTOR('',#6915,0.25);
#1795=VECTOR('',#6918,0.25);
#1796=VECTOR('',#6921,0.25);
#1797=VECTOR('',#6924,0.25);
#1798=VECTOR('',#6937,1.75);
#1799=VECTOR('',#6944,1.);
#1800=VECTOR('',#6955,0.42);
#1801=VECTOR('',#6962,0.8);
#1802=VECTOR('',#6973,1.);
#1803=VECTOR('',#6974,1.);
#1804=VECTOR('',#6975,1.);
#1805=VECTOR('',#6976,1.);
#1806=VECTOR('',#6979,1.);
#1807=VECTOR('',#6980,1.);
#1808=VECTOR('',#6981,1.);
#1809=VECTOR('',#6984,1.);
#1810=VECTOR('',#6985,1.);
#1811=VECTOR('',#6986,1.);
#1812=VECTOR('',#6989,1.);
#1813=VECTOR('',#6990,1.);
#1814=VECTOR('',#6991,1.);
#1815=VECTOR('',#6994,1.);
#1816=VECTOR('',#6995,1.);
#1817=VECTOR('',#6996,1.);
#1818=VECTOR('',#6999,1.);
#1819=VECTOR('',#7000,1.);
#1820=VECTOR('',#7017,0.625);
#1821=VECTOR('',#7022,0.65);
#1822=VECTOR('',#7027,0.635);
#1823=VECTOR('',#7036,0.41);
#1824=VECTOR('',#7039,0.4);
#1825=VECTOR('',#7080,1.);
#1826=VECTOR('',#7081,1.);
#1827=VECTOR('',#7082,1.);
#1828=VECTOR('',#7083,1.);
#1829=VECTOR('',#7088,1.);
#1830=VECTOR('',#7089,1.);
#1831=VECTOR('',#7092,1.);
#1832=VECTOR('',#7093,1.);
#1833=VECTOR('',#7094,1.);
#1834=VECTOR('',#7097,1.);
#1835=VECTOR('',#7106,0.21);
#1836=VECTOR('',#7115,0.21);
#1837=VECTOR('',#7122,1.);
#1838=VECTOR('',#7123,1.);
#1839=VECTOR('',#7124,1.);
#1840=VECTOR('',#7125,1.);
#1841=VECTOR('',#7130,1.);
#1842=VECTOR('',#7131,1.);
#1843=VECTOR('',#7134,1.);
#1844=VECTOR('',#7135,1.);
#1845=VECTOR('',#7136,1.);
#1846=VECTOR('',#7139,1.);
#1847=VECTOR('',#7146,1.);
#1848=VECTOR('',#7147,1.);
#1849=VECTOR('',#7148,1.);
#1850=VECTOR('',#7149,1.);
#1851=VECTOR('',#7154,1.);
#1852=VECTOR('',#7155,1.);
#1853=VECTOR('',#7158,1.);
#1854=VECTOR('',#7159,1.);
#1855=VECTOR('',#7160,1.);
#1856=VECTOR('',#7163,1.);
#1857=VECTOR('',#7172,0.6);
#1858=VECTOR('',#7181,0.6);
#1859=VECTOR('',#7190,1.);
#1860=VECTOR('',#7203,0.605);
#1861=VECTOR('',#7210,0.9);
#1862=VECTOR('',#7223,0.605);
#1863=VECTOR('',#7230,0.9);
#1864=VECTOR('',#7243,0.605);
#1865=VECTOR('',#7250,0.9);
#1866=VECTOR('',#7263,0.275);
#1867=VECTOR('',#7270,1.);
#1868=VECTOR('',#7283,0.275);
#1869=VECTOR('',#7290,1.);
#1870=VECTOR('',#7301,1.);
#1871=VECTOR('',#7308,0.21);
#1872=VECTOR('',#7313,1.);
#1873=VECTOR('',#7316,1.);
#1874=VECTOR('',#7317,1.);
#1875=VECTOR('',#7318,1.);
#1876=VECTOR('',#7319,1.);
#1877=VECTOR('',#7322,1.);
#1878=VECTOR('',#7323,1.);
#1879=VECTOR('',#7324,1.);
#1880=VECTOR('',#7327,1.);
#1881=VECTOR('',#7328,1.);
#1882=VECTOR('',#7329,1.);
#1883=VECTOR('',#7342,2.);
#1884=VECTOR('',#7351,1.);
#1885=VECTOR('',#7358,0.21);
#1886=VECTOR('',#7363,1.);
#1887=VECTOR('',#7368,1.005);
#1888=VECTOR('',#7375,1.5);
#1889=VECTOR('',#7386,1.);
#1890=VECTOR('',#7393,0.21);
#1891=VECTOR('',#7398,1.);
#1892=VECTOR('',#7403,1.005);
#1893=VECTOR('',#7410,1.5);
#1894=VECTOR('',#7421,1.);
#1895=VECTOR('',#7422,1.);
#1896=VECTOR('',#7423,1.);
#1897=VECTOR('',#7424,1.);
#1898=VECTOR('',#7427,1.);
#1899=VECTOR('',#7428,1.);
#1900=VECTOR('',#7429,1.);
#1901=VECTOR('',#7434,1.);
#1902=VECTOR('',#7435,1.);
#1903=VECTOR('',#7436,1.);
#1904=VECTOR('',#7449,0.125);
#1905=VECTOR('',#7452,0.125);
#1906=VECTOR('',#7457,1.);
#1907=VECTOR('',#7458,1.);
#1908=VECTOR('',#7463,0.125);
#1909=VECTOR('',#7466,0.125);
#1910=VECTOR('',#7637,1.4);
#1911=VECTOR('',#7806,1.4);
#1912=VECTOR('',#7809,1.);
#1913=VECTOR('',#7810,1.);
#1914=VECTOR('',#7813,1.);
#1915=VECTOR('',#7816,1.);
#1916=VECTOR('',#7819,1.);
#1917=VECTOR('',#7822,1.);
#1918=VECTOR('',#7825,1.);
#1919=VECTOR('',#7828,1.);
#1920=VECTOR('',#7831,1.);
#1921=VECTOR('',#7834,1.);
#1922=VECTOR('',#7837,1.);
#1923=VECTOR('',#7840,1.);
#1924=VECTOR('',#7843,1.);
#1925=VECTOR('',#7846,1.);
#1926=VECTOR('',#7849,1.);
#1927=VECTOR('',#7852,1.);
#1928=VECTOR('',#7855,1.);
#1929=VECTOR('',#7858,1.);
#1930=VECTOR('',#7861,1.);
#1931=VECTOR('',#7864,1.);
#1932=VECTOR('',#7867,1.);
#1933=VECTOR('',#7870,1.);
#1934=VECTOR('',#7873,1.);
#1935=VECTOR('',#7876,1.);
#1936=VECTOR('',#7879,1.);
#1937=VECTOR('',#7882,1.);
#1938=VECTOR('',#7885,1.);
#1939=VECTOR('',#7888,1.);
#1940=VECTOR('',#7891,1.);
#1941=VECTOR('',#7894,1.);
#1942=VECTOR('',#7897,1.);
#1943=VECTOR('',#7900,1.);
#1944=VECTOR('',#7903,1.);
#1945=VECTOR('',#7906,1.);
#1946=VECTOR('',#7909,1.);
#1947=VECTOR('',#7912,1.);
#1948=VECTOR('',#7915,1.);
#1949=VECTOR('',#7918,1.);
#1950=VECTOR('',#7921,1.);
#1951=VECTOR('',#7924,1.);
#1952=VECTOR('',#7927,1.);
#1953=VECTOR('',#7930,1.);
#1954=VECTOR('',#7933,1.);
#1955=VECTOR('',#7936,1.);
#1956=VECTOR('',#7939,1.);
#1957=VECTOR('',#7942,1.);
#1958=VECTOR('',#7945,1.);
#1959=VECTOR('',#7948,1.);
#1960=VECTOR('',#7951,1.);
#1961=VECTOR('',#7954,1.);
#1962=VECTOR('',#7957,1.);
#1963=VECTOR('',#7960,1.);
#1964=VECTOR('',#7963,1.);
#1965=VECTOR('',#7966,1.);
#1966=VECTOR('',#7969,1.);
#1967=VECTOR('',#7972,1.);
#1968=VECTOR('',#7975,1.);
#1969=VECTOR('',#7978,1.);
#1970=VECTOR('',#7981,1.);
#1971=VECTOR('',#7984,1.);
#1972=VECTOR('',#7987,1.);
#1973=VECTOR('',#7990,1.);
#1974=VECTOR('',#7993,1.);
#1975=VECTOR('',#7996,1.);
#1976=VECTOR('',#7999,1.);
#1977=VECTOR('',#8002,1.);
#1978=VECTOR('',#8005,1.);
#1979=VECTOR('',#8008,1.);
#1980=VECTOR('',#8011,1.);
#1981=VECTOR('',#8014,1.);
#1982=VECTOR('',#8017,1.);
#1983=VECTOR('',#8020,1.);
#1984=VECTOR('',#8023,1.);
#1985=VECTOR('',#8026,1.);
#1986=VECTOR('',#8029,1.);
#1987=VECTOR('',#8032,1.);
#1988=VECTOR('',#8035,1.);
#1989=VECTOR('',#8038,1.);
#1990=VECTOR('',#8041,1.);
#1991=VECTOR('',#8044,1.);
#1992=VECTOR('',#8051,1.);
#1993=VECTOR('',#8052,1.);
#1994=VECTOR('',#8053,1.);
#1995=VECTOR('',#8054,1.);
#1996=VECTOR('',#8055,1.);
#1997=VECTOR('',#8056,1.);
#1998=VECTOR('',#8057,1.);
#1999=VECTOR('',#8058,1.);
#2000=VECTOR('',#8061,1.);
#2001=VECTOR('',#8062,1.);
#2002=VECTOR('',#8063,1.);
#2003=VECTOR('',#8066,1.);
#2004=VECTOR('',#8067,1.);
#2005=VECTOR('',#8070,1.);
#2006=VECTOR('',#8071,1.);
#2007=VECTOR('',#8074,1.);
#2008=VECTOR('',#8075,1.);
#2009=VECTOR('',#8078,1.);
#2010=VECTOR('',#8079,1.);
#2011=VECTOR('',#8080,1.);
#2012=VECTOR('',#8081,1.);
#2013=VECTOR('',#8084,1.);
#2014=VECTOR('',#8087,1.);
#2015=VECTOR('',#8090,1.);
#2016=VECTOR('',#8103,0.4);
#2017=VECTOR('',#8108,0.425);
#2018=VECTOR('',#8113,0.41);
#2019=VECTOR('',#8122,0.26);
#2020=VECTOR('',#8127,0.25);
#2021=VECTOR('',#8132,0.225);
#2022=VECTOR('',#8137,1.);
#2023=VECTOR('',#8138,1.);
#2024=VECTOR('',#8139,1.);
#2025=VECTOR('',#8140,1.);
#2026=VECTOR('',#8143,1.);
#2027=VECTOR('',#8144,1.);
#2028=VECTOR('',#8145,1.);
#2029=VECTOR('',#8148,1.);
#2030=VECTOR('',#8149,1.);
#2031=VECTOR('',#8150,1.);
#2032=VECTOR('',#8153,1.);
#2033=VECTOR('',#8154,1.);
#2034=VECTOR('',#8155,1.);
#2035=VECTOR('',#8158,1.);
#2036=VECTOR('',#8159,1.);
#2037=VECTOR('',#8160,1.);
#2038=VECTOR('',#8163,1.);
#2039=VECTOR('',#8164,1.);
#2040=VECTOR('',#8173,1.);
#2041=VECTOR('',#8174,1.);
#2042=VECTOR('',#8175,1.);
#2043=VECTOR('',#8176,1.);
#2044=VECTOR('',#8177,1.);
#2045=VECTOR('',#8178,1.);
#2046=VECTOR('',#8179,1.);
#2047=VECTOR('',#8180,1.);
#2048=VECTOR('',#8183,1.);
#2049=VECTOR('',#8184,1.);
#2050=VECTOR('',#8185,1.);
#2051=VECTOR('',#8188,1.);
#2052=VECTOR('',#8189,1.);
#2053=VECTOR('',#8192,1.);
#2054=VECTOR('',#8193,1.);
#2055=VECTOR('',#8196,1.);
#2056=VECTOR('',#8197,1.);
#2057=VECTOR('',#8200,1.);
#2058=VECTOR('',#8201,1.);
#2059=VECTOR('',#8202,1.);
#2060=VECTOR('',#8203,1.);
#2061=VECTOR('',#8206,1.);
#2062=VECTOR('',#8209,1.);
#2063=VECTOR('',#8212,1.);
#2064=VECTOR('',#8219,1.);
#2065=VECTOR('',#8220,1.);
#2066=VECTOR('',#8221,1.);
#2067=VECTOR('',#8222,1.);
#2068=VECTOR('',#8225,1.);
#2069=VECTOR('',#8226,1.);
#2070=VECTOR('',#8227,1.);
#2071=VECTOR('',#8230,1.);
#2072=VECTOR('',#8231,1.);
#2073=VECTOR('',#8232,1.);
#2074=VECTOR('',#8235,1.);
#2075=VECTOR('',#8236,1.);
#2076=VECTOR('',#8237,1.);
#2077=VECTOR('',#8240,1.);
#2078=VECTOR('',#8241,1.);
#2079=VECTOR('',#8242,1.);
#2080=VECTOR('',#8245,1.);
#2081=VECTOR('',#8246,1.);
#2082=VECTOR('',#8257,0.235);
#2083=VECTOR('',#8262,0.25);
#2084=VECTOR('',#8267,0.2125);
#2085=CIRCLE('',#5881,0.34);
#2086=CIRCLE('',#5882,0.34);
#2087=CIRCLE('',#5884,0.34);
#2088=CIRCLE('',#5885,0.34);
#2089=CIRCLE('',#5887,0.34);
#2090=CIRCLE('',#5888,0.34);
#2091=CIRCLE('',#5890,0.34);
#2092=CIRCLE('',#5891,0.34);
#2093=CIRCLE('',#5914,0.425);
#2094=CIRCLE('',#5915,0.425);
#2095=CIRCLE('',#5917,0.645);
#2096=CIRCLE('',#5918,0.645);
#2097=CIRCLE('',#5923,0.425);
#2098=CIRCLE('',#5924,0.425);
#2099=CIRCLE('',#5926,0.645);
#2100=CIRCLE('',#5927,0.645);
#2101=CIRCLE('',#5932,0.425);
#2102=CIRCLE('',#5933,0.425);
#2103=CIRCLE('',#5935,0.645);
#2104=CIRCLE('',#5936,0.645);
#2105=CIRCLE('',#5941,0.425);
#2106=CIRCLE('',#5942,0.425);
#2107=CIRCLE('',#5944,0.645);
#2108=CIRCLE('',#5945,0.645);
#2109=CIRCLE('',#5951,2.05);
#2110=CIRCLE('',#5952,2.05);
#2111=CIRCLE('',#5954,2.05);
#2112=CIRCLE('',#5955,2.05);
#2113=CIRCLE('',#5957,2.35);
#2114=CIRCLE('',#5959,2.8);
#2115=CIRCLE('',#5961,2.8);
#2116=CIRCLE('',#5963,2.8);
#2117=CIRCLE('',#5966,2.8);
#2118=CIRCLE('',#5969,0.65);
#2119=CIRCLE('',#5970,0.65);
#2120=CIRCLE('',#5972,2.8);
#2121=CIRCLE('',#5973,2.8);
#2122=CIRCLE('',#5982,0.65);
#2123=CIRCLE('',#5984,0.65);
#2124=CIRCLE('',#5992,1.8);
#2125=CIRCLE('',#5993,1.8);
#2126=CIRCLE('',#5995,2.19089023002066);
#2127=CIRCLE('',#5997,2.35);
#2128=CIRCLE('',#5998,2.19089023002066);
#2129=CIRCLE('',#6003,1.65);
#2130=CIRCLE('',#6004,1.65);
#2131=CIRCLE('',#6010,1.);
#2132=CIRCLE('',#6012,1.75);
#2133=CIRCLE('',#6014,1.75);
#2134=CIRCLE('',#6016,1.);
#2135=CIRCLE('',#6022,0.42);
#2136=CIRCLE('',#6023,0.42);
#2137=CIRCLE('',#6025,0.8);
#2138=CIRCLE('',#6026,0.8);
#2139=CIRCLE('',#6039,0.3933);
#2140=CIRCLE('',#6041,0.6);
#2141=CIRCLE('',#6043,0.65);
#2142=CIRCLE('',#6045,0.65);
#2143=CIRCLE('',#6047,0.62);
#2144=CIRCLE('',#6049,0.42);
#2145=CIRCLE('',#6051,0.3933);
#2146=CIRCLE('',#6074,1.);
#2147=CIRCLE('',#6078,1.);
#2148=CIRCLE('',#6080,0.21);
#2149=CIRCLE('',#6081,0.21);
#2150=CIRCLE('',#6084,0.21);
#2151=CIRCLE('',#6085,0.21);
#2152=CIRCLE('',#6089,0.6);
#2153=CIRCLE('',#6093,0.6);
#2154=CIRCLE('',#6096,0.6);
#2155=CIRCLE('',#6100,0.6);
#2156=CIRCLE('',#6102,0.6);
#2157=CIRCLE('',#6103,0.6);
#2158=CIRCLE('',#6106,0.6);
#2159=CIRCLE('',#6107,0.6);
#2160=CIRCLE('',#6110,1.);
#2161=CIRCLE('',#6111,1.);
#2162=CIRCLE('',#6116,0.605);
#2163=CIRCLE('',#6117,0.605);
#2164=CIRCLE('',#6119,0.9);
#2165=CIRCLE('',#6120,0.9);
#2166=CIRCLE('',#6125,0.605);
#2167=CIRCLE('',#6126,0.605);
#2168=CIRCLE('',#6128,0.9);
#2169=CIRCLE('',#6129,0.9);
#2170=CIRCLE('',#6134,0.605);
#2171=CIRCLE('',#6135,0.605);
#2172=CIRCLE('',#6137,0.9);
#2173=CIRCLE('',#6138,0.9);
#2174=CIRCLE('',#6143,0.275);
#2175=CIRCLE('',#6144,0.275);
#2176=CIRCLE('',#6146,1.);
#2177=CIRCLE('',#6147,1.);
#2178=CIRCLE('',#6152,0.275);
#2179=CIRCLE('',#6153,0.275);
#2180=CIRCLE('',#6155,1.);
#2181=CIRCLE('',#6156,1.);
#2182=CIRCLE('',#6161,0.21);
#2183=CIRCLE('',#6163,0.21);
#2184=CIRCLE('',#6164,0.21);
#2185=CIRCLE('',#6170,2.);
#2186=CIRCLE('',#6171,1.);
#2187=CIRCLE('',#6173,1.);
#2188=CIRCLE('',#6175,2.);
#2189=CIRCLE('',#6179,0.21);
#2190=CIRCLE('',#6181,0.21);
#2191=CIRCLE('',#6182,0.21);
#2192=CIRCLE('',#6185,1.005);
#2193=CIRCLE('',#6186,1.005);
#2194=CIRCLE('',#6188,1.5);
#2195=CIRCLE('',#6189,1.5);
#2196=CIRCLE('',#6194,0.21);
#2197=CIRCLE('',#6196,0.21);
#2198=CIRCLE('',#6197,0.21);
#2199=CIRCLE('',#6200,1.005);
#2200=CIRCLE('',#6201,1.005);
#2201=CIRCLE('',#6203,1.5);
#2202=CIRCLE('',#6204,1.5);
#2203=CIRCLE('',#6210,0.125);
#2204=CIRCLE('',#6213,1.4);
#2205=CIRCLE('',#6214,0.6);
#2206=CIRCLE('',#6216,0.6);
#2207=CIRCLE('',#6220,1.);
#2208=CIRCLE('',#6221,1.);
#2209=CIRCLE('',#6226,1.4);
#2210=CIRCLE('',#6227,0.0555000000000001);
#2211=CIRCLE('',#6228,1.24783954473516);
#2212=CIRCLE('',#6229,0.0555000000000001);
#2213=CIRCLE('',#6230,1.24783954473516);
#2214=CIRCLE('',#6231,0.0555000000000001);
#2215=CIRCLE('',#6232,1.24783954473516);
#2216=CIRCLE('',#6233,0.0555000000000001);
#2217=CIRCLE('',#6234,1.24783954473516);
#2218=CIRCLE('',#6235,0.0555000000000001);
#2219=CIRCLE('',#6236,1.24783954473516);
#2220=CIRCLE('',#6237,0.0555000000000001);
#2221=CIRCLE('',#6238,1.24783954473516);
#2222=CIRCLE('',#6239,0.0555000000000001);
#2223=CIRCLE('',#6240,1.24783954473516);
#2224=CIRCLE('',#6241,0.0555000000000001);
#2225=CIRCLE('',#6242,1.24783954473516);
#2226=CIRCLE('',#6243,0.0555000000000001);
#2227=CIRCLE('',#6244,1.24783954473516);
#2228=CIRCLE('',#6245,0.0555000000000001);
#2229=CIRCLE('',#6246,1.24783954473516);
#2230=CIRCLE('',#6247,0.0555000000000001);
#2231=CIRCLE('',#6248,1.24783954473516);
#2232=CIRCLE('',#6249,0.0555000000000001);
#2233=CIRCLE('',#6250,1.24783954473516);
#2234=CIRCLE('',#6251,0.0555000000000001);
#2235=CIRCLE('',#6252,1.24783954473516);
#2236=CIRCLE('',#6253,0.0555000000000001);
#2237=CIRCLE('',#6254,1.24783954473516);
#2238=CIRCLE('',#6255,0.0555000000000001);
#2239=CIRCLE('',#6256,1.24783954473516);
#2240=CIRCLE('',#6257,0.0555000000000001);
#2241=CIRCLE('',#6258,1.24783954473516);
#2242=CIRCLE('',#6259,0.0555000000000001);
#2243=CIRCLE('',#6260,1.24783954473516);
#2244=CIRCLE('',#6261,0.0555000000000001);
#2245=CIRCLE('',#6262,1.24783954473516);
#2246=CIRCLE('',#6263,0.0555000000000001);
#2247=CIRCLE('',#6264,1.24783954473516);
#2248=CIRCLE('',#6265,0.0555000000000001);
#2249=CIRCLE('',#6266,1.24783954473516);
#2250=CIRCLE('',#6267,0.0555000000000001);
#2251=CIRCLE('',#6268,1.24783954473516);
#2252=CIRCLE('',#6269,0.0555000000000001);
#2253=CIRCLE('',#6270,1.24783954473516);
#2254=CIRCLE('',#6271,0.0555000000000001);
#2255=CIRCLE('',#6272,1.24783954473516);
#2256=CIRCLE('',#6273,0.0555000000000001);
#2257=CIRCLE('',#6274,1.24783954473516);
#2258=CIRCLE('',#6275,0.0555000000000001);
#2259=CIRCLE('',#6276,1.24783954473516);
#2260=CIRCLE('',#6277,0.0555000000000001);
#2261=CIRCLE('',#6278,1.24783954473516);
#2262=CIRCLE('',#6279,0.0555000000000001);
#2263=CIRCLE('',#6280,1.24783954473516);
#2264=CIRCLE('',#6281,0.0555000000000001);
#2265=CIRCLE('',#6282,1.24783954473516);
#2266=CIRCLE('',#6283,0.0555000000000001);
#2267=CIRCLE('',#6284,1.24783954473516);
#2268=CIRCLE('',#6285,0.0555000000000001);
#2269=CIRCLE('',#6286,1.24783954473516);
#2270=CIRCLE('',#6287,0.0555000000000001);
#2271=CIRCLE('',#6288,1.24783954473516);
#2272=CIRCLE('',#6289,0.0555000000000001);
#2273=CIRCLE('',#6290,1.24783954473516);
#2274=CIRCLE('',#6291,0.0555000000000001);
#2275=CIRCLE('',#6292,1.24783954473516);
#2276=CIRCLE('',#6293,0.0555000000000001);
#2277=CIRCLE('',#6294,1.24783954473516);
#2278=CIRCLE('',#6295,0.0555000000000001);
#2279=CIRCLE('',#6296,1.24783954473516);
#2280=CIRCLE('',#6297,0.0555000000000001);
#2281=CIRCLE('',#6298,1.24783954473516);
#2282=CIRCLE('',#6299,0.0555000000000001);
#2283=CIRCLE('',#6300,1.24783954473516);
#2284=CIRCLE('',#6301,0.0555000000000001);
#2285=CIRCLE('',#6302,1.24783954473516);
#2286=CIRCLE('',#6303,0.0555000000000001);
#2287=CIRCLE('',#6304,1.24783954473516);
#2288=CIRCLE('',#6305,0.0555000000000001);
#2289=CIRCLE('',#6306,1.24783954473516);
#2290=CIRCLE('',#6308,1.4);
#2291=CIRCLE('',#6311,1.4);
#2292=CIRCLE('',#6312,0.0555000000000001);
#2293=CIRCLE('',#6313,1.24783954473516);
#2294=CIRCLE('',#6314,0.0555000000000001);
#2295=CIRCLE('',#6315,1.24783954473516);
#2296=CIRCLE('',#6316,0.0555000000000001);
#2297=CIRCLE('',#6317,1.24783954473516);
#2298=CIRCLE('',#6318,0.0555000000000001);
#2299=CIRCLE('',#6319,1.24783954473516);
#2300=CIRCLE('',#6320,0.0555000000000001);
#2301=CIRCLE('',#6321,1.24783954473516);
#2302=CIRCLE('',#6322,0.0555000000000001);
#2303=CIRCLE('',#6323,1.24783954473516);
#2304=CIRCLE('',#6324,0.0555000000000001);
#2305=CIRCLE('',#6325,1.24783954473516);
#2306=CIRCLE('',#6326,0.0555000000000001);
#2307=CIRCLE('',#6327,1.24783954473516);
#2308=CIRCLE('',#6328,0.0555000000000001);
#2309=CIRCLE('',#6329,1.24783954473516);
#2310=CIRCLE('',#6330,0.0555000000000001);
#2311=CIRCLE('',#6331,1.24783954473516);
#2312=CIRCLE('',#6332,0.0555000000000001);
#2313=CIRCLE('',#6333,1.24783954473516);
#2314=CIRCLE('',#6334,0.0555000000000001);
#2315=CIRCLE('',#6335,1.24783954473516);
#2316=CIRCLE('',#6336,0.0555000000000001);
#2317=CIRCLE('',#6337,1.24783954473516);
#2318=CIRCLE('',#6338,0.0555000000000001);
#2319=CIRCLE('',#6339,1.24783954473516);
#2320=CIRCLE('',#6340,0.0555000000000001);
#2321=CIRCLE('',#6341,1.24783954473516);
#2322=CIRCLE('',#6342,0.0555000000000001);
#2323=CIRCLE('',#6343,1.24783954473516);
#2324=CIRCLE('',#6344,0.0555000000000001);
#2325=CIRCLE('',#6345,1.24783954473516);
#2326=CIRCLE('',#6346,0.0555000000000001);
#2327=CIRCLE('',#6347,1.24783954473516);
#2328=CIRCLE('',#6348,0.0555000000000001);
#2329=CIRCLE('',#6349,1.24783954473516);
#2330=CIRCLE('',#6350,0.0555000000000001);
#2331=CIRCLE('',#6351,1.24783954473516);
#2332=CIRCLE('',#6352,0.0555000000000001);
#2333=CIRCLE('',#6353,1.24783954473516);
#2334=CIRCLE('',#6354,0.0555000000000001);
#2335=CIRCLE('',#6355,1.24783954473516);
#2336=CIRCLE('',#6356,0.0555000000000001);
#2337=CIRCLE('',#6357,1.24783954473516);
#2338=CIRCLE('',#6358,0.0555000000000001);
#2339=CIRCLE('',#6359,1.24783954473516);
#2340=CIRCLE('',#6360,0.0555000000000001);
#2341=CIRCLE('',#6361,1.24783954473516);
#2342=CIRCLE('',#6362,0.0555000000000001);
#2343=CIRCLE('',#6363,1.24783954473516);
#2344=CIRCLE('',#6364,0.0555000000000001);
#2345=CIRCLE('',#6365,1.24783954473516);
#2346=CIRCLE('',#6366,0.0555000000000001);
#2347=CIRCLE('',#6367,1.24783954473516);
#2348=CIRCLE('',#6368,0.0555000000000001);
#2349=CIRCLE('',#6369,1.24783954473516);
#2350=CIRCLE('',#6370,0.0555000000000001);
#2351=CIRCLE('',#6371,1.24783954473516);
#2352=CIRCLE('',#6372,0.0555000000000001);
#2353=CIRCLE('',#6373,1.24783954473516);
#2354=CIRCLE('',#6374,0.0555000000000001);
#2355=CIRCLE('',#6375,1.24783954473516);
#2356=CIRCLE('',#6376,0.0555000000000001);
#2357=CIRCLE('',#6377,1.24783954473516);
#2358=CIRCLE('',#6378,0.0555000000000001);
#2359=CIRCLE('',#6379,1.24783954473516);
#2360=CIRCLE('',#6380,0.0555000000000001);
#2361=CIRCLE('',#6381,1.24783954473516);
#2362=CIRCLE('',#6382,0.0555000000000001);
#2363=CIRCLE('',#6383,1.24783954473516);
#2364=CIRCLE('',#6384,0.0555000000000001);
#2365=CIRCLE('',#6385,1.24783954473516);
#2366=CIRCLE('',#6386,0.0555000000000001);
#2367=CIRCLE('',#6387,1.24783954473516);
#2368=CIRCLE('',#6388,0.0555000000000001);
#2369=CIRCLE('',#6389,1.24783954473516);
#2370=CIRCLE('',#6390,0.0555000000000001);
#2371=CIRCLE('',#6391,1.24783954473516);
#2372=CIRCLE('',#6486,0.375);
#2373=CIRCLE('',#6488,0.425);
#2374=CIRCLE('',#6490,0.425);
#2375=CIRCLE('',#6492,0.395);
#2376=CIRCLE('',#6494,0.27);
#2377=CIRCLE('',#6496,0.24505);
#2378=CIRCLE('',#6498,0.24505);
#2379=CIRCLE('',#6500,0.2);
#2380=CIRCLE('',#6530,0.22);
#2381=CIRCLE('',#6532,0.24505);
#2382=CIRCLE('',#6534,0.24505);
#2383=CIRCLE('',#6536,0.175);
#2384=VERTEX_POINT('',#8316);
#2385=VERTEX_POINT('',#8318);
#2386=VERTEX_POINT('',#8322);
#2387=VERTEX_POINT('',#8324);
#2388=VERTEX_POINT('',#8328);
#2389=VERTEX_POINT('',#8330);
#2390=VERTEX_POINT('',#8334);
#2391=VERTEX_POINT('',#8336);
#2392=VERTEX_POINT('',#8340);
#2393=VERTEX_POINT('',#8341);
#2394=VERTEX_POINT('',#8343);
#2395=VERTEX_POINT('',#8345);
#2396=VERTEX_POINT('',#8349);
#2397=VERTEX_POINT('',#8351);
#2398=VERTEX_POINT('',#8355);
#2399=VERTEX_POINT('',#8357);
#2400=VERTEX_POINT('',#8367);
#2401=VERTEX_POINT('',#8368);
#2402=VERTEX_POINT('',#8370);
#2403=VERTEX_POINT('',#8372);
#2404=VERTEX_POINT('',#8376);
#2405=VERTEX_POINT('',#8378);
#2406=VERTEX_POINT('',#8382);
#2407=VERTEX_POINT('',#8384);
#2408=VERTEX_POINT('',#8394);
#2409=VERTEX_POINT('',#8395);
#2410=VERTEX_POINT('',#8397);
#2411=VERTEX_POINT('',#8399);
#2412=VERTEX_POINT('',#8403);
#2413=VERTEX_POINT('',#8405);
#2414=VERTEX_POINT('',#8409);
#2415=VERTEX_POINT('',#8411);
#2416=VERTEX_POINT('',#8421);
#2417=VERTEX_POINT('',#8423);
#2418=VERTEX_POINT('',#8427);
#2419=VERTEX_POINT('',#8429);
#2420=VERTEX_POINT('',#8436);
#2421=VERTEX_POINT('',#8438);
#2422=VERTEX_POINT('',#8442);
#2423=VERTEX_POINT('',#8444);
#2424=VERTEX_POINT('',#8451);
#2425=VERTEX_POINT('',#8453);
#2426=VERTEX_POINT('',#8457);
#2427=VERTEX_POINT('',#8459);
#2428=VERTEX_POINT('',#8466);
#2429=VERTEX_POINT('',#8468);
#2430=VERTEX_POINT('',#8472);
#2431=VERTEX_POINT('',#8474);
#2432=VERTEX_POINT('',#8482);
#2433=VERTEX_POINT('',#8484);
#2434=VERTEX_POINT('',#8488);
#2435=VERTEX_POINT('',#8490);
#2436=VERTEX_POINT('',#8494);
#2437=VERTEX_POINT('',#8495);
#2438=VERTEX_POINT('',#8498);
#2439=VERTEX_POINT('',#8499);
#2440=VERTEX_POINT('',#8501);
#2441=VERTEX_POINT('',#8505);
#2442=VERTEX_POINT('',#8506);
#2443=VERTEX_POINT('',#8508);
#2444=VERTEX_POINT('',#8512);
#2445=VERTEX_POINT('',#8513);
#2446=VERTEX_POINT('',#8515);
#2447=VERTEX_POINT('',#8522);
#2448=VERTEX_POINT('',#8523);
#2449=VERTEX_POINT('',#8525);
#2450=VERTEX_POINT('',#8532);
#2451=VERTEX_POINT('',#8533);
#2452=VERTEX_POINT('',#8535);
#2453=VERTEX_POINT('',#8537);
#2454=VERTEX_POINT('',#8540);
#2455=VERTEX_POINT('',#8542);
#2456=VERTEX_POINT('',#8544);
#2457=VERTEX_POINT('',#8546);
#2458=VERTEX_POINT('',#8549);
#2459=VERTEX_POINT('',#8551);
#2460=VERTEX_POINT('',#8560);
#2461=VERTEX_POINT('',#8561);
#2462=VERTEX_POINT('',#8563);
#2463=VERTEX_POINT('',#8565);
#2464=VERTEX_POINT('',#8569);
#2465=VERTEX_POINT('',#8571);
#2466=VERTEX_POINT('',#8575);
#2467=VERTEX_POINT('',#8577);
#2468=VERTEX_POINT('',#8585);
#2469=VERTEX_POINT('',#8589);
#2470=VERTEX_POINT('',#8593);
#2471=VERTEX_POINT('',#8594);
#2472=VERTEX_POINT('',#8599);
#2473=VERTEX_POINT('',#8603);
#2474=VERTEX_POINT('',#8611);
#2475=VERTEX_POINT('',#8613);
#2476=VERTEX_POINT('',#8617);
#2477=VERTEX_POINT('',#8620);
#2478=VERTEX_POINT('',#8621);
#2479=VERTEX_POINT('',#8623);
#2480=VERTEX_POINT('',#8627);
#2481=VERTEX_POINT('',#8628);
#2482=VERTEX_POINT('',#8639);
#2483=VERTEX_POINT('',#8668);
#2484=VERTEX_POINT('',#8705);
#2485=VERTEX_POINT('',#8740);
#2486=VERTEX_POINT('',#8742);
#2487=VERTEX_POINT('',#8753);
#2488=VERTEX_POINT('',#8783);
#2489=VERTEX_POINT('',#8785);
#2490=VERTEX_POINT('',#8788);
#2491=VERTEX_POINT('',#8789);
#2492=VERTEX_POINT('',#8808);
#2493=VERTEX_POINT('',#8829);
#2494=VERTEX_POINT('',#8830);
#2495=VERTEX_POINT('',#8849);
#2496=VERTEX_POINT('',#8870);
#2497=VERTEX_POINT('',#8871);
#2498=VERTEX_POINT('',#8890);
#2499=VERTEX_POINT('',#8911);
#2500=VERTEX_POINT('',#8912);
#2501=VERTEX_POINT('',#8931);
#2502=VERTEX_POINT('',#8953);
#2503=VERTEX_POINT('',#8990);
#2504=VERTEX_POINT('',#9027);
#2505=VERTEX_POINT('',#9064);
#2506=VERTEX_POINT('',#9101);
#2507=VERTEX_POINT('',#9104);
#2508=VERTEX_POINT('',#9107);
#2509=VERTEX_POINT('',#9111);
#2510=VERTEX_POINT('',#9119);
#2511=VERTEX_POINT('',#9121);
#2512=VERTEX_POINT('',#9125);
#2513=VERTEX_POINT('',#9127);
#2514=VERTEX_POINT('',#9134);
#2515=VERTEX_POINT('',#9135);
#2516=VERTEX_POINT('',#9137);
#2517=VERTEX_POINT('',#9139);
#2518=VERTEX_POINT('',#9143);
#2519=VERTEX_POINT('',#9145);
#2520=VERTEX_POINT('',#9149);
#2521=VERTEX_POINT('',#9151);
#2522=VERTEX_POINT('',#9155);
#2523=VERTEX_POINT('',#9157);
#2524=VERTEX_POINT('',#9161);
#2525=VERTEX_POINT('',#9163);
#2526=VERTEX_POINT('',#9172);
#2527=VERTEX_POINT('',#9175);
#2528=VERTEX_POINT('',#9178);
#2529=VERTEX_POINT('',#9182);
#2530=VERTEX_POINT('',#9186);
#2531=VERTEX_POINT('',#9190);
#2532=VERTEX_POINT('',#9193);
#2533=VERTEX_POINT('',#9218);
#2534=VERTEX_POINT('',#9219);
#2535=VERTEX_POINT('',#9221);
#2536=VERTEX_POINT('',#9223);
#2537=VERTEX_POINT('',#9227);
#2538=VERTEX_POINT('',#9229);
#2539=VERTEX_POINT('',#9233);
#2540=VERTEX_POINT('',#9235);
#2541=VERTEX_POINT('',#9243);
#2542=VERTEX_POINT('',#9245);
#2543=VERTEX_POINT('',#9250);
#2544=VERTEX_POINT('',#9252);
#2545=VERTEX_POINT('',#9257);
#2546=VERTEX_POINT('',#9258);
#2547=VERTEX_POINT('',#9260);
#2548=VERTEX_POINT('',#9262);
#2549=VERTEX_POINT('',#9266);
#2550=VERTEX_POINT('',#9268);
#2551=VERTEX_POINT('',#9272);
#2552=VERTEX_POINT('',#9274);
#2553=VERTEX_POINT('',#9282);
#2554=VERTEX_POINT('',#9283);
#2555=VERTEX_POINT('',#9285);
#2556=VERTEX_POINT('',#9287);
#2557=VERTEX_POINT('',#9291);
#2558=VERTEX_POINT('',#9293);
#2559=VERTEX_POINT('',#9297);
#2560=VERTEX_POINT('',#9299);
#2561=VERTEX_POINT('',#9307);
#2562=VERTEX_POINT('',#9309);
#2563=VERTEX_POINT('',#9314);
#2564=VERTEX_POINT('',#9316);
#2565=VERTEX_POINT('',#9321);
#2566=VERTEX_POINT('',#9323);
#2567=VERTEX_POINT('',#9330);
#2568=VERTEX_POINT('',#9332);
#2569=VERTEX_POINT('',#9336);
#2570=VERTEX_POINT('',#9338);
#2571=VERTEX_POINT('',#9345);
#2572=VERTEX_POINT('',#9347);
#2573=VERTEX_POINT('',#9351);
#2574=VERTEX_POINT('',#9353);
#2575=VERTEX_POINT('',#9360);
#2576=VERTEX_POINT('',#9362);
#2577=VERTEX_POINT('',#9366);
#2578=VERTEX_POINT('',#9368);
#2579=VERTEX_POINT('',#9375);
#2580=VERTEX_POINT('',#9377);
#2581=VERTEX_POINT('',#9381);
#2582=VERTEX_POINT('',#9383);
#2583=VERTEX_POINT('',#9390);
#2584=VERTEX_POINT('',#9392);
#2585=VERTEX_POINT('',#9396);
#2586=VERTEX_POINT('',#9398);
#2587=VERTEX_POINT('',#9405);
#2588=VERTEX_POINT('',#9406);
#2589=VERTEX_POINT('',#9410);
#2590=VERTEX_POINT('',#9421);
#2591=VERTEX_POINT('',#9423);
#2592=VERTEX_POINT('',#9425);
#2593=VERTEX_POINT('',#9462);
#2594=VERTEX_POINT('',#9477);
#2595=VERTEX_POINT('',#9478);
#2596=VERTEX_POINT('',#9480);
#2597=VERTEX_POINT('',#9482);
#2598=VERTEX_POINT('',#9486);
#2599=VERTEX_POINT('',#9488);
#2600=VERTEX_POINT('',#9492);
#2601=VERTEX_POINT('',#9494);
#2602=VERTEX_POINT('',#9498);
#2603=VERTEX_POINT('',#9504);
#2604=VERTEX_POINT('',#9510);
#2605=VERTEX_POINT('',#9511);
#2606=VERTEX_POINT('',#9515);
#2607=VERTEX_POINT('',#9530);
#2608=VERTEX_POINT('',#9532);
#2609=VERTEX_POINT('',#9534);
#2610=VERTEX_POINT('',#9571);
#2611=VERTEX_POINT('',#9590);
#2612=VERTEX_POINT('',#9592);
#2613=VERTEX_POINT('',#9596);
#2614=VERTEX_POINT('',#9598);
#2615=VERTEX_POINT('',#9605);
#2616=VERTEX_POINT('',#9606);
#2617=VERTEX_POINT('',#9610);
#2618=VERTEX_POINT('',#9625);
#2619=VERTEX_POINT('',#9627);
#2620=VERTEX_POINT('',#9629);
#2621=VERTEX_POINT('',#9666);
#2622=VERTEX_POINT('',#9685);
#2623=VERTEX_POINT('',#9687);
#2624=VERTEX_POINT('',#9691);
#2625=VERTEX_POINT('',#9693);
#2626=VERTEX_POINT('',#9700);
#2627=VERTEX_POINT('',#9701);
#2628=VERTEX_POINT('',#9703);
#2629=VERTEX_POINT('',#9705);
#2630=VERTEX_POINT('',#9709);
#2631=VERTEX_POINT('',#9711);
#2632=VERTEX_POINT('',#9714);
#2633=VERTEX_POINT('',#9717);
#2634=VERTEX_POINT('',#9719);
#2635=VERTEX_POINT('',#9723);
#2636=VERTEX_POINT('',#9728);
#2637=VERTEX_POINT('',#9729);
#2638=VERTEX_POINT('',#9766);
#2639=VERTEX_POINT('',#9767);
#2640=VERTEX_POINT('',#9804);
#2641=VERTEX_POINT('',#9805);
#2642=VERTEX_POINT('',#9843);
#2643=VERTEX_POINT('',#9844);
#2644=VERTEX_POINT('',#9855);
#2645=VERTEX_POINT('',#9886);
#2646=VERTEX_POINT('',#9888);
#2647=VERTEX_POINT('',#9899);
#2648=VERTEX_POINT('',#9929);
#2649=VERTEX_POINT('',#9932);
#2650=VERTEX_POINT('',#9935);
#2651=VERTEX_POINT('',#9936);
#2652=VERTEX_POINT('',#9955);
#2653=VERTEX_POINT('',#9976);
#2654=VERTEX_POINT('',#9977);
#2655=VERTEX_POINT('',#9996);
#2656=VERTEX_POINT('',#10023);
#2657=VERTEX_POINT('',#10025);
#2658=VERTEX_POINT('',#10026);
#2659=VERTEX_POINT('',#10028);
#2660=VERTEX_POINT('',#10030);
#2661=VERTEX_POINT('',#10032);
#2662=VERTEX_POINT('',#10034);
#2663=VERTEX_POINT('',#10036);
#2664=VERTEX_POINT('',#10038);
#2665=VERTEX_POINT('',#10040);
#2666=VERTEX_POINT('',#10042);
#2667=VERTEX_POINT('',#10044);
#2668=VERTEX_POINT('',#10046);
#2669=VERTEX_POINT('',#10048);
#2670=VERTEX_POINT('',#10050);
#2671=VERTEX_POINT('',#10052);
#2672=VERTEX_POINT('',#10054);
#2673=VERTEX_POINT('',#10056);
#2674=VERTEX_POINT('',#10058);
#2675=VERTEX_POINT('',#10060);
#2676=VERTEX_POINT('',#10062);
#2677=VERTEX_POINT('',#10064);
#2678=VERTEX_POINT('',#10066);
#2679=VERTEX_POINT('',#10068);
#2680=VERTEX_POINT('',#10070);
#2681=VERTEX_POINT('',#10072);
#2682=VERTEX_POINT('',#10074);
#2683=VERTEX_POINT('',#10076);
#2684=VERTEX_POINT('',#10078);
#2685=VERTEX_POINT('',#10080);
#2686=VERTEX_POINT('',#10082);
#2687=VERTEX_POINT('',#10084);
#2688=VERTEX_POINT('',#10086);
#2689=VERTEX_POINT('',#10088);
#2690=VERTEX_POINT('',#10090);
#2691=VERTEX_POINT('',#10092);
#2692=VERTEX_POINT('',#10094);
#2693=VERTEX_POINT('',#10096);
#2694=VERTEX_POINT('',#10098);
#2695=VERTEX_POINT('',#10100);
#2696=VERTEX_POINT('',#10102);
#2697=VERTEX_POINT('',#10104);
#2698=VERTEX_POINT('',#10106);
#2699=VERTEX_POINT('',#10108);
#2700=VERTEX_POINT('',#10110);
#2701=VERTEX_POINT('',#10112);
#2702=VERTEX_POINT('',#10114);
#2703=VERTEX_POINT('',#10116);
#2704=VERTEX_POINT('',#10118);
#2705=VERTEX_POINT('',#10120);
#2706=VERTEX_POINT('',#10122);
#2707=VERTEX_POINT('',#10124);
#2708=VERTEX_POINT('',#10126);
#2709=VERTEX_POINT('',#10128);
#2710=VERTEX_POINT('',#10130);
#2711=VERTEX_POINT('',#10132);
#2712=VERTEX_POINT('',#10134);
#2713=VERTEX_POINT('',#10136);
#2714=VERTEX_POINT('',#10138);
#2715=VERTEX_POINT('',#10140);
#2716=VERTEX_POINT('',#10142);
#2717=VERTEX_POINT('',#10144);
#2718=VERTEX_POINT('',#10146);
#2719=VERTEX_POINT('',#10148);
#2720=VERTEX_POINT('',#10150);
#2721=VERTEX_POINT('',#10152);
#2722=VERTEX_POINT('',#10154);
#2723=VERTEX_POINT('',#10156);
#2724=VERTEX_POINT('',#10158);
#2725=VERTEX_POINT('',#10160);
#2726=VERTEX_POINT('',#10162);
#2727=VERTEX_POINT('',#10164);
#2728=VERTEX_POINT('',#10166);
#2729=VERTEX_POINT('',#10168);
#2730=VERTEX_POINT('',#10170);
#2731=VERTEX_POINT('',#10172);
#2732=VERTEX_POINT('',#10174);
#2733=VERTEX_POINT('',#10176);
#2734=VERTEX_POINT('',#10178);
#2735=VERTEX_POINT('',#10180);
#2736=VERTEX_POINT('',#10182);
#2737=VERTEX_POINT('',#10186);
#2738=VERTEX_POINT('',#10191);
#2739=VERTEX_POINT('',#10193);
#2740=VERTEX_POINT('',#10194);
#2741=VERTEX_POINT('',#10196);
#2742=VERTEX_POINT('',#10198);
#2743=VERTEX_POINT('',#10200);
#2744=VERTEX_POINT('',#10202);
#2745=VERTEX_POINT('',#10204);
#2746=VERTEX_POINT('',#10206);
#2747=VERTEX_POINT('',#10208);
#2748=VERTEX_POINT('',#10210);
#2749=VERTEX_POINT('',#10212);
#2750=VERTEX_POINT('',#10214);
#2751=VERTEX_POINT('',#10216);
#2752=VERTEX_POINT('',#10218);
#2753=VERTEX_POINT('',#10220);
#2754=VERTEX_POINT('',#10222);
#2755=VERTEX_POINT('',#10224);
#2756=VERTEX_POINT('',#10226);
#2757=VERTEX_POINT('',#10228);
#2758=VERTEX_POINT('',#10230);
#2759=VERTEX_POINT('',#10232);
#2760=VERTEX_POINT('',#10234);
#2761=VERTEX_POINT('',#10236);
#2762=VERTEX_POINT('',#10238);
#2763=VERTEX_POINT('',#10240);
#2764=VERTEX_POINT('',#10242);
#2765=VERTEX_POINT('',#10244);
#2766=VERTEX_POINT('',#10246);
#2767=VERTEX_POINT('',#10248);
#2768=VERTEX_POINT('',#10250);
#2769=VERTEX_POINT('',#10252);
#2770=VERTEX_POINT('',#10254);
#2771=VERTEX_POINT('',#10256);
#2772=VERTEX_POINT('',#10258);
#2773=VERTEX_POINT('',#10260);
#2774=VERTEX_POINT('',#10262);
#2775=VERTEX_POINT('',#10264);
#2776=VERTEX_POINT('',#10266);
#2777=VERTEX_POINT('',#10268);
#2778=VERTEX_POINT('',#10270);
#2779=VERTEX_POINT('',#10272);
#2780=VERTEX_POINT('',#10274);
#2781=VERTEX_POINT('',#10276);
#2782=VERTEX_POINT('',#10278);
#2783=VERTEX_POINT('',#10280);
#2784=VERTEX_POINT('',#10282);
#2785=VERTEX_POINT('',#10284);
#2786=VERTEX_POINT('',#10286);
#2787=VERTEX_POINT('',#10288);
#2788=VERTEX_POINT('',#10290);
#2789=VERTEX_POINT('',#10292);
#2790=VERTEX_POINT('',#10294);
#2791=VERTEX_POINT('',#10296);
#2792=VERTEX_POINT('',#10298);
#2793=VERTEX_POINT('',#10300);
#2794=VERTEX_POINT('',#10302);
#2795=VERTEX_POINT('',#10304);
#2796=VERTEX_POINT('',#10306);
#2797=VERTEX_POINT('',#10308);
#2798=VERTEX_POINT('',#10310);
#2799=VERTEX_POINT('',#10312);
#2800=VERTEX_POINT('',#10314);
#2801=VERTEX_POINT('',#10316);
#2802=VERTEX_POINT('',#10318);
#2803=VERTEX_POINT('',#10320);
#2804=VERTEX_POINT('',#10322);
#2805=VERTEX_POINT('',#10324);
#2806=VERTEX_POINT('',#10326);
#2807=VERTEX_POINT('',#10328);
#2808=VERTEX_POINT('',#10330);
#2809=VERTEX_POINT('',#10332);
#2810=VERTEX_POINT('',#10334);
#2811=VERTEX_POINT('',#10336);
#2812=VERTEX_POINT('',#10338);
#2813=VERTEX_POINT('',#10340);
#2814=VERTEX_POINT('',#10342);
#2815=VERTEX_POINT('',#10344);
#2816=VERTEX_POINT('',#10346);
#2817=VERTEX_POINT('',#10348);
#2818=VERTEX_POINT('',#10350);
#2819=VERTEX_POINT('',#10517);
#2820=VERTEX_POINT('',#10518);
#2821=VERTEX_POINT('',#10520);
#2822=VERTEX_POINT('',#10522);
#2823=VERTEX_POINT('',#10524);
#2824=VERTEX_POINT('',#10526);
#2825=VERTEX_POINT('',#10528);
#2826=VERTEX_POINT('',#10530);
#2827=VERTEX_POINT('',#10534);
#2828=VERTEX_POINT('',#10536);
#2829=VERTEX_POINT('',#10540);
#2830=VERTEX_POINT('',#10544);
#2831=VERTEX_POINT('',#10548);
#2832=VERTEX_POINT('',#10552);
#2833=VERTEX_POINT('',#10554);
#2834=VERTEX_POINT('',#10556);
#2835=VERTEX_POINT('',#10568);
#2836=VERTEX_POINT('',#10571);
#2837=VERTEX_POINT('',#10575);
#2838=VERTEX_POINT('',#10579);
#2839=VERTEX_POINT('',#10583);
#2840=VERTEX_POINT('',#10586);
#2841=VERTEX_POINT('',#10590);
#2842=VERTEX_POINT('',#10594);
#2843=VERTEX_POINT('',#10599);
#2844=VERTEX_POINT('',#10600);
#2845=VERTEX_POINT('',#10602);
#2846=VERTEX_POINT('',#10604);
#2847=VERTEX_POINT('',#10608);
#2848=VERTEX_POINT('',#10610);
#2849=VERTEX_POINT('',#10614);
#2850=VERTEX_POINT('',#10616);
#2851=VERTEX_POINT('',#10620);
#2852=VERTEX_POINT('',#10622);
#2853=VERTEX_POINT('',#10626);
#2854=VERTEX_POINT('',#10628);
#2855=VERTEX_POINT('',#10638);
#2856=VERTEX_POINT('',#10639);
#2857=VERTEX_POINT('',#10641);
#2858=VERTEX_POINT('',#10643);
#2859=VERTEX_POINT('',#10645);
#2860=VERTEX_POINT('',#10647);
#2861=VERTEX_POINT('',#10649);
#2862=VERTEX_POINT('',#10651);
#2863=VERTEX_POINT('',#10655);
#2864=VERTEX_POINT('',#10657);
#2865=VERTEX_POINT('',#10661);
#2866=VERTEX_POINT('',#10665);
#2867=VERTEX_POINT('',#10669);
#2868=VERTEX_POINT('',#10673);
#2869=VERTEX_POINT('',#10674);
#2870=VERTEX_POINT('',#10677);
#2871=VERTEX_POINT('',#10689);
#2872=VERTEX_POINT('',#10690);
#2873=VERTEX_POINT('',#10692);
#2874=VERTEX_POINT('',#10694);
#2875=VERTEX_POINT('',#10698);
#2876=VERTEX_POINT('',#10700);
#2877=VERTEX_POINT('',#10704);
#2878=VERTEX_POINT('',#10706);
#2879=VERTEX_POINT('',#10710);
#2880=VERTEX_POINT('',#10712);
#2881=VERTEX_POINT('',#10716);
#2882=VERTEX_POINT('',#10718);
#2883=VERTEX_POINT('',#10726);
#2884=VERTEX_POINT('',#10729);
#2885=VERTEX_POINT('',#10733);
#2886=VERTEX_POINT('',#10737);
#2887=EDGE_CURVE('',#2384,#2384,#2085,.T.);
#2888=EDGE_CURVE('',#2384,#2385,#1307,.T.);
#2889=EDGE_CURVE('',#2385,#2385,#2086,.T.);
#2890=EDGE_CURVE('',#2386,#2386,#2087,.T.);
#2891=EDGE_CURVE('',#2386,#2387,#1308,.T.);
#2892=EDGE_CURVE('',#2387,#2387,#2088,.T.);
#2893=EDGE_CURVE('',#2388,#2388,#2089,.T.);
#2894=EDGE_CURVE('',#2388,#2389,#1309,.T.);
#2895=EDGE_CURVE('',#2389,#2389,#2090,.T.);
#2896=EDGE_CURVE('',#2390,#2390,#2091,.T.);
#2897=EDGE_CURVE('',#2390,#2391,#1310,.T.);
#2898=EDGE_CURVE('',#2391,#2391,#2092,.T.);
#2899=EDGE_CURVE('',#2392,#2393,#1311,.T.);
#2900=EDGE_CURVE('',#2393,#2394,#1312,.T.);
#2901=EDGE_CURVE('',#2395,#2394,#1313,.T.);
#2902=EDGE_CURVE('',#2392,#2395,#1314,.T.);
#2903=EDGE_CURVE('',#2396,#2392,#1315,.T.);
#2904=EDGE_CURVE('',#2397,#2395,#1316,.T.);
#2905=EDGE_CURVE('',#2396,#2397,#1317,.T.);
#2906=EDGE_CURVE('',#2398,#2396,#1318,.T.);
#2907=EDGE_CURVE('',#2399,#2397,#1319,.T.);
#2908=EDGE_CURVE('',#2398,#2399,#1320,.T.);
#2909=EDGE_CURVE('',#2393,#2398,#1321,.T.);
#2910=EDGE_CURVE('',#2394,#2399,#1322,.T.);
#2911=EDGE_CURVE('',#2400,#2401,#1323,.T.);
#2912=EDGE_CURVE('',#2401,#2402,#1324,.T.);
#2913=EDGE_CURVE('',#2403,#2402,#1325,.T.);
#2914=EDGE_CURVE('',#2400,#2403,#1326,.T.);
#2915=EDGE_CURVE('',#2404,#2400,#1327,.T.);
#2916=EDGE_CURVE('',#2405,#2403,#1328,.T.);
#2917=EDGE_CURVE('',#2404,#2405,#1329,.T.);
#2918=EDGE_CURVE('',#2406,#2404,#1330,.T.);
#2919=EDGE_CURVE('',#2407,#2405,#1331,.T.);
#2920=EDGE_CURVE('',#2406,#2407,#1332,.T.);
#2921=EDGE_CURVE('',#2401,#2406,#1333,.T.);
#2922=EDGE_CURVE('',#2402,#2407,#1334,.T.);
#2923=EDGE_CURVE('',#2408,#2409,#1335,.T.);
#2924=EDGE_CURVE('',#2409,#2410,#1336,.T.);
#2925=EDGE_CURVE('',#2411,#2410,#1337,.T.);
#2926=EDGE_CURVE('',#2408,#2411,#1338,.T.);
#2927=EDGE_CURVE('',#2412,#2408,#1339,.T.);
#2928=EDGE_CURVE('',#2413,#2411,#1340,.T.);
#2929=EDGE_CURVE('',#2412,#2413,#1341,.T.);
#2930=EDGE_CURVE('',#2414,#2412,#1342,.T.);
#2931=EDGE_CURVE('',#2415,#2413,#1343,.T.);
#2932=EDGE_CURVE('',#2414,#2415,#1344,.T.);
#2933=EDGE_CURVE('',#2409,#2414,#1345,.T.);
#2934=EDGE_CURVE('',#2410,#2415,#1346,.T.);
#2935=EDGE_CURVE('',#2416,#2416,#2093,.T.);
#2936=EDGE_CURVE('',#2416,#2417,#1347,.T.);
#2937=EDGE_CURVE('',#2417,#2417,#2094,.T.);
#2938=EDGE_CURVE('',#2418,#2418,#2095,.T.);
#2939=EDGE_CURVE('',#2418,#2419,#1348,.T.);
#2940=EDGE_CURVE('',#2419,#2419,#2096,.T.);
#2941=EDGE_CURVE('',#2420,#2420,#2097,.T.);
#2942=EDGE_CURVE('',#2420,#2421,#1349,.T.);
#2943=EDGE_CURVE('',#2421,#2421,#2098,.T.);
#2944=EDGE_CURVE('',#2422,#2422,#2099,.T.);
#2945=EDGE_CURVE('',#2422,#2423,#1350,.T.);
#2946=EDGE_CURVE('',#2423,#2423,#2100,.T.);
#2947=EDGE_CURVE('',#2424,#2424,#2101,.T.);
#2948=EDGE_CURVE('',#2424,#2425,#1351,.T.);
#2949=EDGE_CURVE('',#2425,#2425,#2102,.T.);
#2950=EDGE_CURVE('',#2426,#2426,#2103,.T.);
#2951=EDGE_CURVE('',#2426,#2427,#1352,.T.);
#2952=EDGE_CURVE('',#2427,#2427,#2104,.T.);
#2953=EDGE_CURVE('',#2428,#2428,#2105,.T.);
#2954=EDGE_CURVE('',#2428,#2429,#1353,.T.);
#2955=EDGE_CURVE('',#2429,#2429,#2106,.T.);
#2956=EDGE_CURVE('',#2430,#2430,#2107,.T.);
#2957=EDGE_CURVE('',#2430,#2431,#1354,.T.);
#2958=EDGE_CURVE('',#2431,#2431,#2108,.T.);
#2959=EDGE_CURVE('',#2432,#2432,#2109,.T.);
#2960=EDGE_CURVE('',#2432,#2433,#1355,.T.);
#2961=EDGE_CURVE('',#2433,#2433,#2110,.T.);
#2962=EDGE_CURVE('',#2434,#2434,#2111,.T.);
#2963=EDGE_CURVE('',#2434,#2435,#1356,.T.);
#2964=EDGE_CURVE('',#2435,#2435,#2112,.T.);
#2965=EDGE_CURVE('',#2436,#2437,#2113,.T.);
#2966=EDGE_CURVE('',#2438,#2439,#1357,.T.);
#2967=EDGE_CURVE('',#2438,#2440,#1358,.T.);
#2968=EDGE_CURVE('',#2439,#2440,#2114,.T.);
#2969=EDGE_CURVE('',#2441,#2442,#1359,.T.);
#2970=EDGE_CURVE('',#2443,#2441,#2115,.T.);
#2971=EDGE_CURVE('',#2443,#2442,#1360,.T.);
#2972=EDGE_CURVE('',#2444,#2445,#1361,.T.);
#2973=EDGE_CURVE('',#2446,#2444,#2116,.T.);
#2974=EDGE_CURVE('',#2446,#2445,#1362,.T.);
#2975=EDGE_CURVE('',#2445,#2438,#1363,.T.);
#2976=EDGE_CURVE('',#2440,#2446,#1364,.T.);
#2977=EDGE_CURVE('',#2447,#2448,#1365,.T.);
#2978=EDGE_CURVE('',#2447,#2449,#1366,.T.);
#2979=EDGE_CURVE('',#2448,#2449,#2117,.T.);
#2980=EDGE_CURVE('',#2442,#2447,#1367,.T.);
#2981=EDGE_CURVE('',#2449,#2443,#1368,.T.);
#2982=EDGE_CURVE('',#2450,#2451,#1369,.T.);
#2983=EDGE_CURVE('',#2451,#2452,#1370,.T.);
#2984=EDGE_CURVE('',#2452,#2453,#1371,.T.);
#2985=EDGE_CURVE('',#2453,#2450,#1372,.T.);
#2986=EDGE_CURVE('',#2454,#2454,#2118,.T.);
#2987=EDGE_CURVE('',#2455,#2455,#2119,.T.);
#2988=EDGE_CURVE('',#2448,#2456,#1373,.T.);
#2989=EDGE_CURVE('',#2456,#2457,#1374,.T.);
#2990=EDGE_CURVE('',#2457,#2444,#1375,.T.);
#2991=EDGE_CURVE('',#2439,#2458,#1376,.T.);
#2992=EDGE_CURVE('',#2458,#2459,#1377,.T.);
#2993=EDGE_CURVE('',#2459,#2441,#1378,.T.);
#2994=EDGE_CURVE('',#2458,#2459,#2120,.T.);
#2995=EDGE_CURVE('',#2456,#2457,#2121,.T.);
#2996=EDGE_CURVE('',#2460,#2461,#1379,.T.);
#2997=EDGE_CURVE('',#2460,#2462,#1380,.T.);
#2998=EDGE_CURVE('',#2462,#2463,#1381,.T.);
#2999=EDGE_CURVE('',#2461,#2463,#1382,.T.);
#3000=EDGE_CURVE('',#2464,#2460,#1383,.T.);
#3001=EDGE_CURVE('',#2464,#2465,#1384,.T.);
#3002=EDGE_CURVE('',#2465,#2462,#1385,.T.);
#3003=EDGE_CURVE('',#2466,#2464,#1386,.T.);
#3004=EDGE_CURVE('',#2466,#2467,#1387,.T.);
#3005=EDGE_CURVE('',#2467,#2465,#1388,.T.);
#3006=EDGE_CURVE('',#2461,#2466,#1389,.T.);
#3007=EDGE_CURVE('',#2463,#2467,#1390,.T.);
#3008=EDGE_CURVE('',#2468,#2468,#2122,.T.);
#3009=EDGE_CURVE('',#2468,#2455,#1391,.T.);
#3010=EDGE_CURVE('',#2469,#2469,#2123,.T.);
#3011=EDGE_CURVE('',#2469,#2454,#1392,.T.);
#3012=EDGE_CURVE('',#2470,#2471,#1393,.T.);
#3013=EDGE_CURVE('',#2471,#2450,#1394,.T.);
#3014=EDGE_CURVE('',#2470,#2453,#1395,.T.);
#3015=EDGE_CURVE('',#2472,#2470,#1396,.T.);
#3016=EDGE_CURVE('',#2472,#2452,#1397,.T.);
#3017=EDGE_CURVE('',#2473,#2472,#1398,.T.);
#3018=EDGE_CURVE('',#2473,#2451,#1399,.T.);
#3019=EDGE_CURVE('',#2471,#2473,#1400,.T.);
#3020=EDGE_CURVE('',#2474,#2474,#2124,.T.);
#3021=EDGE_CURVE('',#2474,#2475,#1401,.T.);
#3022=EDGE_CURVE('',#2475,#2475,#2125,.T.);
#3023=EDGE_CURVE('',#2476,#2476,#2126,.T.);
#3024=EDGE_CURVE('',#2477,#2478,#2127,.T.);
#3025=EDGE_CURVE('',#2479,#2479,#2128,.T.);
#3026=EDGE_CURVE('',#2480,#2481,#184,.T.);
#3027=EDGE_CURVE('',#2482,#2480,#185,.T.);
#3028=EDGE_CURVE('',#2481,#2482,#186,.T.);
#3029=EDGE_CURVE('',#2481,#2483,#1402,.T.);
#3030=EDGE_CURVE('',#2483,#2483,#187,.T.);
#3031=EDGE_CURVE('',#2484,#2484,#188,.T.);
#3032=EDGE_CURVE('',#2484,#2485,#1403,.T.);
#3033=EDGE_CURVE('',#2486,#2485,#189,.T.);
#3034=EDGE_CURVE('',#2487,#2486,#190,.T.);
#3035=EDGE_CURVE('',#2485,#2487,#191,.T.);
#3036=EDGE_CURVE('',#2488,#2488,#2129,.T.);
#3037=EDGE_CURVE('',#2488,#2489,#1404,.T.);
#3038=EDGE_CURVE('',#2489,#2489,#2130,.T.);
#3039=EDGE_CURVE('',#2490,#2491,#192,.T.);
#3040=EDGE_CURVE('',#2491,#2492,#193,.T.);
#3041=EDGE_CURVE('',#2492,#2490,#194,.T.);
#3042=EDGE_CURVE('',#2493,#2494,#195,.T.);
#3043=EDGE_CURVE('',#2494,#2495,#196,.T.);
#3044=EDGE_CURVE('',#2495,#2493,#197,.T.);
#3045=EDGE_CURVE('',#2496,#2497,#198,.T.);
#3046=EDGE_CURVE('',#2497,#2498,#199,.T.);
#3047=EDGE_CURVE('',#2498,#2496,#200,.T.);
#3048=EDGE_CURVE('',#2499,#2500,#201,.T.);
#3049=EDGE_CURVE('',#2500,#2501,#202,.T.);
#3050=EDGE_CURVE('',#2501,#2499,#203,.T.);
#3051=EDGE_CURVE('',#2492,#2502,#1405,.T.);
#3052=EDGE_CURVE('',#2502,#2502,#204,.T.);
#3053=EDGE_CURVE('',#2503,#2503,#205,.T.);
#3054=EDGE_CURVE('',#2503,#2495,#1406,.T.);
#3055=EDGE_CURVE('',#2498,#2504,#1407,.T.);
#3056=EDGE_CURVE('',#2504,#2504,#206,.T.);
#3057=EDGE_CURVE('',#2505,#2505,#207,.T.);
#3058=EDGE_CURVE('',#2505,#2501,#1408,.T.);
#3059=EDGE_CURVE('',#2506,#2506,#2131,.T.);
#3060=EDGE_CURVE('',#2507,#2507,#2132,.T.);
#3061=EDGE_CURVE('',#2508,#2508,#2133,.T.);
#3062=EDGE_CURVE('',#2508,#2507,#1409,.T.);
#3063=EDGE_CURVE('',#2509,#2509,#2134,.T.);
#3064=EDGE_CURVE('',#2509,#2506,#1410,.T.);
#3065=EDGE_CURVE('',#2510,#2510,#2135,.T.);
#3066=EDGE_CURVE('',#2510,#2511,#1411,.T.);
#3067=EDGE_CURVE('',#2511,#2511,#2136,.T.);
#3068=EDGE_CURVE('',#2512,#2512,#2137,.T.);
#3069=EDGE_CURVE('',#2512,#2513,#1412,.T.);
#3070=EDGE_CURVE('',#2513,#2513,#2138,.T.);
#3071=EDGE_CURVE('',#2514,#2515,#1413,.T.);
#3072=EDGE_CURVE('',#2515,#2516,#1414,.T.);
#3073=EDGE_CURVE('',#2516,#2517,#1415,.T.);
#3074=EDGE_CURVE('',#2514,#2517,#1416,.T.);
#3075=EDGE_CURVE('',#2515,#2518,#1417,.T.);
#3076=EDGE_CURVE('',#2518,#2519,#1418,.T.);
#3077=EDGE_CURVE('',#2519,#2516,#1419,.T.);
#3078=EDGE_CURVE('',#2518,#2520,#1420,.T.);
#3079=EDGE_CURVE('',#2520,#2521,#1421,.T.);
#3080=EDGE_CURVE('',#2521,#2519,#1422,.T.);
#3081=EDGE_CURVE('',#2520,#2522,#1423,.T.);
#3082=EDGE_CURVE('',#2522,#2523,#1424,.T.);
#3083=EDGE_CURVE('',#2523,#2521,#1425,.T.);
#3084=EDGE_CURVE('',#2522,#2524,#1426,.T.);
#3085=EDGE_CURVE('',#2524,#2525,#1427,.T.);
#3086=EDGE_CURVE('',#2525,#2523,#1428,.T.);
#3087=EDGE_CURVE('',#2524,#2514,#1429,.T.);
#3088=EDGE_CURVE('',#2517,#2525,#1430,.T.);
#3089=EDGE_CURVE('',#2526,#2526,#2139,.T.);
#3090=EDGE_CURVE('',#2527,#2527,#2140,.T.);
#3091=EDGE_CURVE('',#2528,#2528,#2141,.T.);
#3092=EDGE_CURVE('',#2528,#2527,#1431,.T.);
#3093=EDGE_CURVE('',#2529,#2529,#2142,.T.);
#3094=EDGE_CURVE('',#2529,#2528,#1432,.T.);
#3095=EDGE_CURVE('',#2530,#2530,#2143,.T.);
#3096=EDGE_CURVE('',#2530,#2529,#1433,.T.);
#3097=EDGE_CURVE('',#2531,#2531,#2144,.T.);
#3098=EDGE_CURVE('',#2532,#2532,#2145,.F.);
#3099=EDGE_CURVE('',#2532,#2531,#1434,.T.);
#3100=EDGE_CURVE('',#2526,#2532,#1435,.T.);
#3101=EDGE_CURVE('',#2533,#2534,#1436,.T.);
#3102=EDGE_CURVE('',#2533,#2535,#1437,.T.);
#3103=EDGE_CURVE('',#2536,#2535,#1438,.T.);
#3104=EDGE_CURVE('',#2536,#2534,#1439,.T.);
#3105=EDGE_CURVE('',#2534,#2537,#2146,.T.);
#3106=EDGE_CURVE('',#2538,#2536,#1440,.T.);
#3107=EDGE_CURVE('',#2537,#2538,#1441,.T.);
#3108=EDGE_CURVE('',#2537,#2539,#1442,.T.);
#3109=EDGE_CURVE('',#2538,#2540,#1443,.T.);
#3110=EDGE_CURVE('',#2540,#2539,#1444,.T.);
#3111=EDGE_CURVE('',#2535,#2540,#1445,.T.);
#3112=EDGE_CURVE('',#2539,#2533,#2147,.T.);
#3113=EDGE_CURVE('',#2541,#2541,#2148,.T.);
#3114=EDGE_CURVE('',#2541,#2542,#1446,.T.);
#3115=EDGE_CURVE('',#2542,#2542,#2149,.T.);
#3116=EDGE_CURVE('',#2543,#2543,#2150,.T.);
#3117=EDGE_CURVE('',#2543,#2544,#1447,.T.);
#3118=EDGE_CURVE('',#2544,#2544,#2151,.T.);
#3119=EDGE_CURVE('',#2545,#2546,#1448,.T.);
#3120=EDGE_CURVE('',#2545,#2547,#1449,.T.);
#3121=EDGE_CURVE('',#2548,#2547,#1450,.T.);
#3122=EDGE_CURVE('',#2548,#2546,#1451,.T.);
#3123=EDGE_CURVE('',#2546,#2549,#2152,.T.);
#3124=EDGE_CURVE('',#2550,#2548,#1452,.T.);
#3125=EDGE_CURVE('',#2549,#2550,#1453,.T.);
#3126=EDGE_CURVE('',#2549,#2551,#1454,.T.);
#3127=EDGE_CURVE('',#2550,#2552,#1455,.T.);
#3128=EDGE_CURVE('',#2552,#2551,#1456,.T.);
#3129=EDGE_CURVE('',#2547,#2552,#1457,.T.);
#3130=EDGE_CURVE('',#2551,#2545,#2153,.T.);
#3131=EDGE_CURVE('',#2553,#2554,#1458,.T.);
#3132=EDGE_CURVE('',#2553,#2555,#1459,.T.);
#3133=EDGE_CURVE('',#2556,#2555,#1460,.T.);
#3134=EDGE_CURVE('',#2556,#2554,#1461,.T.);
#3135=EDGE_CURVE('',#2554,#2557,#2154,.T.);
#3136=EDGE_CURVE('',#2558,#2556,#1462,.T.);
#3137=EDGE_CURVE('',#2557,#2558,#1463,.T.);
#3138=EDGE_CURVE('',#2557,#2559,#1464,.T.);
#3139=EDGE_CURVE('',#2558,#2560,#1465,.T.);
#3140=EDGE_CURVE('',#2560,#2559,#1466,.T.);
#3141=EDGE_CURVE('',#2555,#2560,#1467,.T.);
#3142=EDGE_CURVE('',#2559,#2553,#2155,.T.);
#3143=EDGE_CURVE('',#2561,#2561,#2156,.T.);
#3144=EDGE_CURVE('',#2561,#2562,#1468,.T.);
#3145=EDGE_CURVE('',#2562,#2562,#2157,.T.);
#3146=EDGE_CURVE('',#2563,#2563,#2158,.T.);
#3147=EDGE_CURVE('',#2563,#2564,#1469,.T.);
#3148=EDGE_CURVE('',#2564,#2564,#2159,.T.);
#3149=EDGE_CURVE('',#2565,#2565,#2160,.T.);
#3150=EDGE_CURVE('',#2565,#2566,#1470,.T.);
#3151=EDGE_CURVE('',#2566,#2566,#2161,.T.);
#3152=EDGE_CURVE('',#2567,#2567,#2162,.T.);
#3153=EDGE_CURVE('',#2567,#2568,#1471,.T.);
#3154=EDGE_CURVE('',#2568,#2568,#2163,.T.);
#3155=EDGE_CURVE('',#2569,#2569,#2164,.T.);
#3156=EDGE_CURVE('',#2569,#2570,#1472,.T.);
#3157=EDGE_CURVE('',#2570,#2570,#2165,.T.);
#3158=EDGE_CURVE('',#2571,#2571,#2166,.T.);
#3159=EDGE_CURVE('',#2571,#2572,#1473,.T.);
#3160=EDGE_CURVE('',#2572,#2572,#2167,.T.);
#3161=EDGE_CURVE('',#2573,#2573,#2168,.T.);
#3162=EDGE_CURVE('',#2573,#2574,#1474,.T.);
#3163=EDGE_CURVE('',#2574,#2574,#2169,.T.);
#3164=EDGE_CURVE('',#2575,#2575,#2170,.T.);
#3165=EDGE_CURVE('',#2575,#2576,#1475,.T.);
#3166=EDGE_CURVE('',#2576,#2576,#2171,.T.);
#3167=EDGE_CURVE('',#2577,#2577,#2172,.T.);
#3168=EDGE_CURVE('',#2577,#2578,#1476,.T.);
#3169=EDGE_CURVE('',#2578,#2578,#2173,.T.);
#3170=EDGE_CURVE('',#2579,#2579,#2174,.T.);
#3171=EDGE_CURVE('',#2579,#2580,#1477,.T.);
#3172=EDGE_CURVE('',#2580,#2580,#2175,.T.);
#3173=EDGE_CURVE('',#2581,#2581,#2176,.T.);
#3174=EDGE_CURVE('',#2581,#2582,#1478,.T.);
#3175=EDGE_CURVE('',#2582,#2582,#2177,.T.);
#3176=EDGE_CURVE('',#2583,#2583,#2178,.T.);
#3177=EDGE_CURVE('',#2583,#2584,#1479,.T.);
#3178=EDGE_CURVE('',#2584,#2584,#2179,.T.);
#3179=EDGE_CURVE('',#2585,#2585,#2180,.T.);
#3180=EDGE_CURVE('',#2585,#2586,#1480,.T.);
#3181=EDGE_CURVE('',#2586,#2586,#2181,.T.);
#3182=EDGE_CURVE('',#2587,#2588,#1481,.T.);
#3183=EDGE_CURVE('',#2587,#2588,#2182,.T.);
#3184=EDGE_CURVE('',#2589,#2587,#208,.T.);
#3185=EDGE_CURVE('',#2590,#2589,#2183,.T.);
#3186=EDGE_CURVE('',#2590,#2591,#1482,.T.);
#3187=EDGE_CURVE('',#2592,#2591,#209,.T.);
#3188=EDGE_CURVE('',#2591,#2592,#210,.T.);
#3189=EDGE_CURVE('',#2593,#2590,#2184,.T.);
#3190=EDGE_CURVE('',#2588,#2593,#211,.T.);
#3191=EDGE_CURVE('',#2593,#2589,#1483,.T.);
#3192=EDGE_CURVE('',#2594,#2595,#1484,.T.);
#3193=EDGE_CURVE('',#2594,#2596,#1485,.T.);
#3194=EDGE_CURVE('',#2597,#2596,#1486,.T.);
#3195=EDGE_CURVE('',#2595,#2597,#1487,.T.);
#3196=EDGE_CURVE('',#2598,#2594,#1488,.T.);
#3197=EDGE_CURVE('',#2598,#2599,#1489,.T.);
#3198=EDGE_CURVE('',#2596,#2599,#1490,.T.);
#3199=EDGE_CURVE('',#2600,#2598,#1491,.T.);
#3200=EDGE_CURVE('',#2601,#2600,#1492,.T.);
#3201=EDGE_CURVE('',#2599,#2601,#1493,.T.);
#3202=EDGE_CURVE('',#2602,#2602,#2185,.T.);
#3203=EDGE_CURVE('',#2601,#2597,#2186,.T.);
#3204=EDGE_CURVE('',#2600,#2595,#2187,.T.);
#3205=EDGE_CURVE('',#2602,#2603,#1494,.T.);
#3206=EDGE_CURVE('',#2603,#2603,#2188,.T.);
#3207=EDGE_CURVE('',#2604,#2605,#1495,.T.);
#3208=EDGE_CURVE('',#2604,#2605,#2189,.T.);
#3209=EDGE_CURVE('',#2606,#2604,#212,.T.);
#3210=EDGE_CURVE('',#2607,#2606,#2190,.T.);
#3211=EDGE_CURVE('',#2607,#2608,#1496,.T.);
#3212=EDGE_CURVE('',#2609,#2608,#213,.T.);
#3213=EDGE_CURVE('',#2608,#2609,#214,.T.);
#3214=EDGE_CURVE('',#2610,#2607,#2191,.T.);
#3215=EDGE_CURVE('',#2605,#2610,#215,.T.);
#3216=EDGE_CURVE('',#2610,#2606,#1497,.T.);
#3217=EDGE_CURVE('',#2611,#2611,#2192,.T.);
#3218=EDGE_CURVE('',#2611,#2612,#1498,.T.);
#3219=EDGE_CURVE('',#2612,#2612,#2193,.T.);
#3220=EDGE_CURVE('',#2613,#2613,#2194,.T.);
#3221=EDGE_CURVE('',#2613,#2614,#1499,.T.);
#3222=EDGE_CURVE('',#2614,#2614,#2195,.T.);
#3223=EDGE_CURVE('',#2615,#2616,#1500,.T.);
#3224=EDGE_CURVE('',#2615,#2616,#2196,.T.);
#3225=EDGE_CURVE('',#2617,#2615,#216,.T.);
#3226=EDGE_CURVE('',#2618,#2617,#2197,.T.);
#3227=EDGE_CURVE('',#2618,#2619,#1501,.T.);
#3228=EDGE_CURVE('',#2620,#2619,#217,.T.);
#3229=EDGE_CURVE('',#2619,#2620,#218,.T.);
#3230=EDGE_CURVE('',#2621,#2618,#2198,.T.);
#3231=EDGE_CURVE('',#2616,#2621,#219,.T.);
#3232=EDGE_CURVE('',#2621,#2617,#1502,.T.);
#3233=EDGE_CURVE('',#2622,#2622,#2199,.T.);
#3234=EDGE_CURVE('',#2622,#2623,#1503,.T.);
#3235=EDGE_CURVE('',#2623,#2623,#2200,.T.);
#3236=EDGE_CURVE('',#2624,#2624,#2201,.T.);
#3237=EDGE_CURVE('',#2624,#2625,#1504,.T.);
#3238=EDGE_CURVE('',#2625,#2625,#2202,.T.);
#3239=EDGE_CURVE('',#2626,#2627,#1505,.T.);
#3240=EDGE_CURVE('',#2626,#2628,#1506,.T.);
#3241=EDGE_CURVE('',#2629,#2628,#1507,.T.);
#3242=EDGE_CURVE('',#2627,#2629,#1508,.T.);
#3243=EDGE_CURVE('',#2630,#2626,#1509,.T.);
#3244=EDGE_CURVE('',#2630,#2631,#1510,.T.);
#3245=EDGE_CURVE('',#2628,#2631,#1511,.T.);
#3246=EDGE_CURVE('',#2632,#2632,#2203,.T.);
#3247=EDGE_CURVE('',#2633,#2630,#1512,.T.);
#3248=EDGE_CURVE('',#2634,#2633,#1513,.T.);
#3249=EDGE_CURVE('',#2631,#2634,#1514,.T.);
#3250=EDGE_CURVE('',#2635,#2635,#2204,.T.);
#3251=EDGE_CURVE('',#2634,#2629,#2205,.T.);
#3252=EDGE_CURVE('',#2627,#2633,#2206,.T.);
#3253=EDGE_CURVE('',#2636,#2637,#220,.T.);
#3254=EDGE_CURVE('',#2637,#2636,#221,.T.);
#3255=EDGE_CURVE('',#2638,#2639,#222,.T.);
#3256=EDGE_CURVE('',#2639,#2638,#223,.T.);
#3257=EDGE_CURVE('',#2640,#2641,#224,.T.);
#3258=EDGE_CURVE('',#2641,#2640,#225,.T.);
#3259=EDGE_CURVE('',#2642,#2643,#226,.T.);
#3260=EDGE_CURVE('',#2644,#2642,#227,.T.);
#3261=EDGE_CURVE('',#2643,#2644,#228,.T.);
#3262=EDGE_CURVE('',#2643,#2639,#1515,.T.);
#3263=EDGE_CURVE('',#2641,#2645,#1516,.T.);
#3264=EDGE_CURVE('',#2646,#2645,#229,.T.);
#3265=EDGE_CURVE('',#2647,#2646,#230,.T.);
#3266=EDGE_CURVE('',#2645,#2647,#231,.T.);
#3267=EDGE_CURVE('',#2648,#2648,#2207,.T.);
#3268=EDGE_CURVE('',#2648,#2644,#1517,.T.);
#3269=EDGE_CURVE('',#2642,#2649,#1518,.T.);
#3270=EDGE_CURVE('',#2649,#2649,#2208,.T.);
#3271=EDGE_CURVE('',#2650,#2651,#232,.T.);
#3272=EDGE_CURVE('',#2651,#2652,#233,.T.);
#3273=EDGE_CURVE('',#2652,#2650,#234,.T.);
#3274=EDGE_CURVE('',#2653,#2654,#235,.T.);
#3275=EDGE_CURVE('',#2654,#2655,#236,.T.);
#3276=EDGE_CURVE('',#2655,#2653,#237,.T.);
#3277=EDGE_CURVE('',#2652,#2632,#1519,.T.);
#3278=EDGE_CURVE('',#2637,#2655,#1520,.T.);
#3279=EDGE_CURVE('',#2656,#2656,#2209,.T.);
#3280=EDGE_CURVE('',#2657,#2658,#2210,.T.);
#3281=EDGE_CURVE('',#2659,#2658,#2211,.T.);
#3282=EDGE_CURVE('',#2659,#2660,#2212,.T.);
#3283=EDGE_CURVE('',#2661,#2660,#2213,.T.);
#3284=EDGE_CURVE('',#2661,#2662,#2214,.T.);
#3285=EDGE_CURVE('',#2663,#2662,#2215,.T.);
#3286=EDGE_CURVE('',#2663,#2664,#2216,.T.);
#3287=EDGE_CURVE('',#2665,#2664,#2217,.T.);
#3288=EDGE_CURVE('',#2665,#2666,#2218,.T.);
#3289=EDGE_CURVE('',#2667,#2666,#2219,.T.);
#3290=EDGE_CURVE('',#2667,#2668,#2220,.T.);
#3291=EDGE_CURVE('',#2669,#2668,#2221,.T.);
#3292=EDGE_CURVE('',#2669,#2670,#2222,.T.);
#3293=EDGE_CURVE('',#2671,#2670,#2223,.T.);
#3294=EDGE_CURVE('',#2671,#2672,#2224,.T.);
#3295=EDGE_CURVE('',#2673,#2672,#2225,.T.);
#3296=EDGE_CURVE('',#2673,#2674,#2226,.T.);
#3297=EDGE_CURVE('',#2675,#2674,#2227,.T.);
#3298=EDGE_CURVE('',#2675,#2676,#2228,.T.);
#3299=EDGE_CURVE('',#2677,#2676,#2229,.T.);
#3300=EDGE_CURVE('',#2677,#2678,#2230,.T.);
#3301=EDGE_CURVE('',#2679,#2678,#2231,.T.);
#3302=EDGE_CURVE('',#2679,#2680,#2232,.T.);
#3303=EDGE_CURVE('',#2681,#2680,#2233,.T.);
#3304=EDGE_CURVE('',#2681,#2682,#2234,.T.);
#3305=EDGE_CURVE('',#2683,#2682,#2235,.T.);
#3306=EDGE_CURVE('',#2683,#2684,#2236,.T.);
#3307=EDGE_CURVE('',#2685,#2684,#2237,.T.);
#3308=EDGE_CURVE('',#2685,#2686,#2238,.T.);
#3309=EDGE_CURVE('',#2687,#2686,#2239,.T.);
#3310=EDGE_CURVE('',#2687,#2688,#2240,.T.);
#3311=EDGE_CURVE('',#2689,#2688,#2241,.T.);
#3312=EDGE_CURVE('',#2689,#2690,#2242,.T.);
#3313=EDGE_CURVE('',#2691,#2690,#2243,.T.);
#3314=EDGE_CURVE('',#2691,#2692,#2244,.T.);
#3315=EDGE_CURVE('',#2693,#2692,#2245,.T.);
#3316=EDGE_CURVE('',#2693,#2694,#2246,.T.);
#3317=EDGE_CURVE('',#2695,#2694,#2247,.T.);
#3318=EDGE_CURVE('',#2695,#2696,#2248,.T.);
#3319=EDGE_CURVE('',#2697,#2696,#2249,.T.);
#3320=EDGE_CURVE('',#2697,#2698,#2250,.T.);
#3321=EDGE_CURVE('',#2699,#2698,#2251,.T.);
#3322=EDGE_CURVE('',#2699,#2700,#2252,.T.);
#3323=EDGE_CURVE('',#2701,#2700,#2253,.T.);
#3324=EDGE_CURVE('',#2701,#2702,#2254,.T.);
#3325=EDGE_CURVE('',#2703,#2702,#2255,.T.);
#3326=EDGE_CURVE('',#2703,#2704,#2256,.T.);
#3327=EDGE_CURVE('',#2705,#2704,#2257,.T.);
#3328=EDGE_CURVE('',#2705,#2706,#2258,.T.);
#3329=EDGE_CURVE('',#2707,#2706,#2259,.T.);
#3330=EDGE_CURVE('',#2707,#2708,#2260,.T.);
#3331=EDGE_CURVE('',#2709,#2708,#2261,.T.);
#3332=EDGE_CURVE('',#2709,#2710,#2262,.T.);
#3333=EDGE_CURVE('',#2711,#2710,#2263,.T.);
#3334=EDGE_CURVE('',#2711,#2712,#2264,.T.);
#3335=EDGE_CURVE('',#2713,#2712,#2265,.T.);
#3336=EDGE_CURVE('',#2713,#2714,#2266,.T.);
#3337=EDGE_CURVE('',#2715,#2714,#2267,.T.);
#3338=EDGE_CURVE('',#2715,#2716,#2268,.T.);
#3339=EDGE_CURVE('',#2717,#2716,#2269,.T.);
#3340=EDGE_CURVE('',#2717,#2718,#2270,.T.);
#3341=EDGE_CURVE('',#2719,#2718,#2271,.T.);
#3342=EDGE_CURVE('',#2719,#2720,#2272,.T.);
#3343=EDGE_CURVE('',#2721,#2720,#2273,.T.);
#3344=EDGE_CURVE('',#2721,#2722,#2274,.T.);
#3345=EDGE_CURVE('',#2723,#2722,#2275,.T.);
#3346=EDGE_CURVE('',#2723,#2724,#2276,.T.);
#3347=EDGE_CURVE('',#2725,#2724,#2277,.T.);
#3348=EDGE_CURVE('',#2725,#2726,#2278,.T.);
#3349=EDGE_CURVE('',#2727,#2726,#2279,.T.);
#3350=EDGE_CURVE('',#2727,#2728,#2280,.T.);
#3351=EDGE_CURVE('',#2729,#2728,#2281,.T.);
#3352=EDGE_CURVE('',#2729,#2730,#2282,.T.);
#3353=EDGE_CURVE('',#2731,#2730,#2283,.T.);
#3354=EDGE_CURVE('',#2731,#2732,#2284,.T.);
#3355=EDGE_CURVE('',#2733,#2732,#2285,.T.);
#3356=EDGE_CURVE('',#2733,#2734,#2286,.T.);
#3357=EDGE_CURVE('',#2735,#2734,#2287,.T.);
#3358=EDGE_CURVE('',#2735,#2736,#2288,.T.);
#3359=EDGE_CURVE('',#2657,#2736,#2289,.T.);
#3360=EDGE_CURVE('',#2737,#2737,#2290,.T.);
#3361=EDGE_CURVE('',#2737,#2656,#1521,.T.);
#3362=EDGE_CURVE('',#2738,#2738,#2291,.T.);
#3363=EDGE_CURVE('',#2739,#2740,#2292,.T.);
#3364=EDGE_CURVE('',#2740,#2741,#2293,.T.);
#3365=EDGE_CURVE('',#2741,#2742,#2294,.T.);
#3366=EDGE_CURVE('',#2742,#2743,#2295,.T.);
#3367=EDGE_CURVE('',#2743,#2744,#2296,.T.);
#3368=EDGE_CURVE('',#2744,#2745,#2297,.T.);
#3369=EDGE_CURVE('',#2745,#2746,#2298,.T.);
#3370=EDGE_CURVE('',#2746,#2747,#2299,.T.);
#3371=EDGE_CURVE('',#2747,#2748,#2300,.T.);
#3372=EDGE_CURVE('',#2748,#2749,#2301,.T.);
#3373=EDGE_CURVE('',#2749,#2750,#2302,.T.);
#3374=EDGE_CURVE('',#2750,#2751,#2303,.T.);
#3375=EDGE_CURVE('',#2751,#2752,#2304,.T.);
#3376=EDGE_CURVE('',#2752,#2753,#2305,.T.);
#3377=EDGE_CURVE('',#2753,#2754,#2306,.T.);
#3378=EDGE_CURVE('',#2754,#2755,#2307,.T.);
#3379=EDGE_CURVE('',#2755,#2756,#2308,.T.);
#3380=EDGE_CURVE('',#2756,#2757,#2309,.T.);
#3381=EDGE_CURVE('',#2757,#2758,#2310,.T.);
#3382=EDGE_CURVE('',#2758,#2759,#2311,.T.);
#3383=EDGE_CURVE('',#2759,#2760,#2312,.T.);
#3384=EDGE_CURVE('',#2760,#2761,#2313,.T.);
#3385=EDGE_CURVE('',#2761,#2762,#2314,.T.);
#3386=EDGE_CURVE('',#2762,#2763,#2315,.T.);
#3387=EDGE_CURVE('',#2763,#2764,#2316,.T.);
#3388=EDGE_CURVE('',#2764,#2765,#2317,.T.);
#3389=EDGE_CURVE('',#2765,#2766,#2318,.T.);
#3390=EDGE_CURVE('',#2766,#2767,#2319,.T.);
#3391=EDGE_CURVE('',#2767,#2768,#2320,.T.);
#3392=EDGE_CURVE('',#2768,#2769,#2321,.T.);
#3393=EDGE_CURVE('',#2769,#2770,#2322,.T.);
#3394=EDGE_CURVE('',#2770,#2771,#2323,.T.);
#3395=EDGE_CURVE('',#2771,#2772,#2324,.T.);
#3396=EDGE_CURVE('',#2772,#2773,#2325,.T.);
#3397=EDGE_CURVE('',#2773,#2774,#2326,.T.);
#3398=EDGE_CURVE('',#2774,#2775,#2327,.T.);
#3399=EDGE_CURVE('',#2775,#2776,#2328,.T.);
#3400=EDGE_CURVE('',#2776,#2777,#2329,.T.);
#3401=EDGE_CURVE('',#2777,#2778,#2330,.T.);
#3402=EDGE_CURVE('',#2778,#2779,#2331,.T.);
#3403=EDGE_CURVE('',#2779,#2780,#2332,.T.);
#3404=EDGE_CURVE('',#2780,#2781,#2333,.T.);
#3405=EDGE_CURVE('',#2781,#2782,#2334,.T.);
#3406=EDGE_CURVE('',#2782,#2783,#2335,.T.);
#3407=EDGE_CURVE('',#2783,#2784,#2336,.T.);
#3408=EDGE_CURVE('',#2784,#2785,#2337,.T.);
#3409=EDGE_CURVE('',#2785,#2786,#2338,.T.);
#3410=EDGE_CURVE('',#2786,#2787,#2339,.T.);
#3411=EDGE_CURVE('',#2787,#2788,#2340,.T.);
#3412=EDGE_CURVE('',#2788,#2789,#2341,.T.);
#3413=EDGE_CURVE('',#2789,#2790,#2342,.T.);
#3414=EDGE_CURVE('',#2790,#2791,#2343,.T.);
#3415=EDGE_CURVE('',#2791,#2792,#2344,.T.);
#3416=EDGE_CURVE('',#2792,#2793,#2345,.T.);
#3417=EDGE_CURVE('',#2793,#2794,#2346,.T.);
#3418=EDGE_CURVE('',#2794,#2795,#2347,.T.);
#3419=EDGE_CURVE('',#2795,#2796,#2348,.T.);
#3420=EDGE_CURVE('',#2796,#2797,#2349,.T.);
#3421=EDGE_CURVE('',#2797,#2798,#2350,.T.);
#3422=EDGE_CURVE('',#2798,#2799,#2351,.T.);
#3423=EDGE_CURVE('',#2799,#2800,#2352,.T.);
#3424=EDGE_CURVE('',#2800,#2801,#2353,.T.);
#3425=EDGE_CURVE('',#2801,#2802,#2354,.T.);
#3426=EDGE_CURVE('',#2802,#2803,#2355,.T.);
#3427=EDGE_CURVE('',#2803,#2804,#2356,.T.);
#3428=EDGE_CURVE('',#2804,#2805,#2357,.T.);
#3429=EDGE_CURVE('',#2805,#2806,#2358,.T.);
#3430=EDGE_CURVE('',#2806,#2807,#2359,.T.);
#3431=EDGE_CURVE('',#2807,#2808,#2360,.T.);
#3432=EDGE_CURVE('',#2808,#2809,#2361,.T.);
#3433=EDGE_CURVE('',#2809,#2810,#2362,.T.);
#3434=EDGE_CURVE('',#2810,#2811,#2363,.T.);
#3435=EDGE_CURVE('',#2811,#2812,#2364,.T.);
#3436=EDGE_CURVE('',#2812,#2813,#2365,.T.);
#3437=EDGE_CURVE('',#2813,#2814,#2366,.T.);
#3438=EDGE_CURVE('',#2814,#2815,#2367,.T.);
#3439=EDGE_CURVE('',#2815,#2816,#2368,.T.);
#3440=EDGE_CURVE('',#2816,#2817,#2369,.T.);
#3441=EDGE_CURVE('',#2817,#2818,#2370,.T.);
#3442=EDGE_CURVE('',#2818,#2739,#2371,.T.);
#3443=EDGE_CURVE('',#2635,#2738,#1522,.T.);
#3444=EDGE_CURVE('',#2740,#2657,#1523,.T.);
#3445=EDGE_CURVE('',#2658,#2739,#1524,.T.);
#3446=EDGE_CURVE('',#2818,#2659,#1525,.T.);
#3447=EDGE_CURVE('',#2660,#2817,#1526,.T.);
#3448=EDGE_CURVE('',#2816,#2661,#1527,.T.);
#3449=EDGE_CURVE('',#2662,#2815,#1528,.T.);
#3450=EDGE_CURVE('',#2814,#2663,#1529,.T.);
#3451=EDGE_CURVE('',#2664,#2813,#1530,.T.);
#3452=EDGE_CURVE('',#2812,#2665,#1531,.T.);
#3453=EDGE_CURVE('',#2666,#2811,#1532,.T.);
#3454=EDGE_CURVE('',#2810,#2667,#1533,.T.);
#3455=EDGE_CURVE('',#2668,#2809,#1534,.T.);
#3456=EDGE_CURVE('',#2808,#2669,#1535,.T.);
#3457=EDGE_CURVE('',#2670,#2807,#1536,.T.);
#3458=EDGE_CURVE('',#2806,#2671,#1537,.T.);
#3459=EDGE_CURVE('',#2672,#2805,#1538,.T.);
#3460=EDGE_CURVE('',#2804,#2673,#1539,.T.);
#3461=EDGE_CURVE('',#2674,#2803,#1540,.T.);
#3462=EDGE_CURVE('',#2802,#2675,#1541,.T.);
#3463=EDGE_CURVE('',#2676,#2801,#1542,.T.);
#3464=EDGE_CURVE('',#2800,#2677,#1543,.T.);
#3465=EDGE_CURVE('',#2678,#2799,#1544,.T.);
#3466=EDGE_CURVE('',#2798,#2679,#1545,.T.);
#3467=EDGE_CURVE('',#2680,#2797,#1546,.T.);
#3468=EDGE_CURVE('',#2796,#2681,#1547,.T.);
#3469=EDGE_CURVE('',#2682,#2795,#1548,.T.);
#3470=EDGE_CURVE('',#2794,#2683,#1549,.T.);
#3471=EDGE_CURVE('',#2684,#2793,#1550,.T.);
#3472=EDGE_CURVE('',#2792,#2685,#1551,.T.);
#3473=EDGE_CURVE('',#2686,#2791,#1552,.T.);
#3474=EDGE_CURVE('',#2790,#2687,#1553,.T.);
#3475=EDGE_CURVE('',#2688,#2789,#1554,.T.);
#3476=EDGE_CURVE('',#2788,#2689,#1555,.T.);
#3477=EDGE_CURVE('',#2690,#2787,#1556,.T.);
#3478=EDGE_CURVE('',#2786,#2691,#1557,.T.);
#3479=EDGE_CURVE('',#2692,#2785,#1558,.T.);
#3480=EDGE_CURVE('',#2784,#2693,#1559,.T.);
#3481=EDGE_CURVE('',#2694,#2783,#1560,.T.);
#3482=EDGE_CURVE('',#2782,#2695,#1561,.T.);
#3483=EDGE_CURVE('',#2696,#2781,#1562,.T.);
#3484=EDGE_CURVE('',#2780,#2697,#1563,.T.);
#3485=EDGE_CURVE('',#2698,#2779,#1564,.T.);
#3486=EDGE_CURVE('',#2778,#2699,#1565,.T.);
#3487=EDGE_CURVE('',#2700,#2777,#1566,.T.);
#3488=EDGE_CURVE('',#2776,#2701,#1567,.T.);
#3489=EDGE_CURVE('',#2702,#2775,#1568,.T.);
#3490=EDGE_CURVE('',#2774,#2703,#1569,.T.);
#3491=EDGE_CURVE('',#2704,#2773,#1570,.T.);
#3492=EDGE_CURVE('',#2772,#2705,#1571,.T.);
#3493=EDGE_CURVE('',#2706,#2771,#1572,.T.);
#3494=EDGE_CURVE('',#2770,#2707,#1573,.T.);
#3495=EDGE_CURVE('',#2708,#2769,#1574,.T.);
#3496=EDGE_CURVE('',#2768,#2709,#1575,.T.);
#3497=EDGE_CURVE('',#2710,#2767,#1576,.T.);
#3498=EDGE_CURVE('',#2766,#2711,#1577,.T.);
#3499=EDGE_CURVE('',#2712,#2765,#1578,.T.);
#3500=EDGE_CURVE('',#2764,#2713,#1579,.T.);
#3501=EDGE_CURVE('',#2714,#2763,#1580,.T.);
#3502=EDGE_CURVE('',#2762,#2715,#1581,.T.);
#3503=EDGE_CURVE('',#2716,#2761,#1582,.T.);
#3504=EDGE_CURVE('',#2760,#2717,#1583,.T.);
#3505=EDGE_CURVE('',#2718,#2759,#1584,.T.);
#3506=EDGE_CURVE('',#2758,#2719,#1585,.T.);
#3507=EDGE_CURVE('',#2720,#2757,#1586,.T.);
#3508=EDGE_CURVE('',#2756,#2721,#1587,.T.);
#3509=EDGE_CURVE('',#2722,#2755,#1588,.T.);
#3510=EDGE_CURVE('',#2754,#2723,#1589,.T.);
#3511=EDGE_CURVE('',#2724,#2753,#1590,.T.);
#3512=EDGE_CURVE('',#2752,#2725,#1591,.T.);
#3513=EDGE_CURVE('',#2726,#2751,#1592,.T.);
#3514=EDGE_CURVE('',#2750,#2727,#1593,.T.);
#3515=EDGE_CURVE('',#2728,#2749,#1594,.T.);
#3516=EDGE_CURVE('',#2748,#2729,#1595,.T.);
#3517=EDGE_CURVE('',#2730,#2747,#1596,.T.);
#3518=EDGE_CURVE('',#2746,#2731,#1597,.T.);
#3519=EDGE_CURVE('',#2732,#2745,#1598,.T.);
#3520=EDGE_CURVE('',#2744,#2733,#1599,.T.);
#3521=EDGE_CURVE('',#2734,#2743,#1600,.T.);
#3522=EDGE_CURVE('',#2736,#2741,#1601,.T.);
#3523=EDGE_CURVE('',#2742,#2735,#1602,.T.);
#3524=EDGE_CURVE('',#2819,#2820,#1603,.T.);
#3525=EDGE_CURVE('',#2821,#2819,#1604,.T.);
#3526=EDGE_CURVE('',#2822,#2821,#1605,.T.);
#3527=EDGE_CURVE('',#2823,#2822,#1606,.T.);
#3528=EDGE_CURVE('',#2824,#2823,#1607,.T.);
#3529=EDGE_CURVE('',#2825,#2824,#1608,.T.);
#3530=EDGE_CURVE('',#2826,#2825,#1609,.T.);
#3531=EDGE_CURVE('',#2820,#2826,#1610,.T.);
#3532=EDGE_CURVE('',#2823,#2827,#1611,.T.);
#3533=EDGE_CURVE('',#2827,#2828,#1612,.T.);
#3534=EDGE_CURVE('',#2828,#2824,#1613,.T.);
#3535=EDGE_CURVE('',#2829,#2822,#1614,.T.);
#3536=EDGE_CURVE('',#2829,#2827,#1615,.T.);
#3537=EDGE_CURVE('',#2821,#2830,#1616,.T.);
#3538=EDGE_CURVE('',#2830,#2829,#1617,.T.);
#3539=EDGE_CURVE('',#2831,#2819,#1618,.T.);
#3540=EDGE_CURVE('',#2831,#2830,#1619,.T.);
#3541=EDGE_CURVE('',#2832,#2831,#1620,.T.);
#3542=EDGE_CURVE('',#2833,#2832,#1621,.T.);
#3543=EDGE_CURVE('',#2834,#2833,#1622,.T.);
#3544=EDGE_CURVE('',#2828,#2834,#1623,.T.);
#3545=EDGE_CURVE('',#2820,#2832,#1624,.T.);
#3546=EDGE_CURVE('',#2833,#2826,#1625,.T.);
#3547=EDGE_CURVE('',#2825,#2834,#1626,.T.);
#3548=EDGE_CURVE('',#2835,#2835,#2372,.T.);
#3549=EDGE_CURVE('',#2836,#2836,#2373,.T.);
#3550=EDGE_CURVE('',#2836,#2835,#1627,.T.);
#3551=EDGE_CURVE('',#2837,#2837,#2374,.T.);
#3552=EDGE_CURVE('',#2837,#2836,#1628,.T.);
#3553=EDGE_CURVE('',#2838,#2838,#2375,.T.);
#3554=EDGE_CURVE('',#2838,#2837,#1629,.T.);
#3555=EDGE_CURVE('',#2839,#2839,#2376,.T.);
#3556=EDGE_CURVE('',#2840,#2840,#2377,.F.);
#3557=EDGE_CURVE('',#2840,#2839,#1630,.T.);
#3558=EDGE_CURVE('',#2841,#2841,#2378,.F.);
#3559=EDGE_CURVE('',#2841,#2840,#1631,.T.);
#3560=EDGE_CURVE('',#2842,#2842,#2379,.T.);
#3561=EDGE_CURVE('',#2842,#2841,#1632,.T.);
#3562=EDGE_CURVE('',#2843,#2844,#1633,.T.);
#3563=EDGE_CURVE('',#2844,#2845,#1634,.T.);
#3564=EDGE_CURVE('',#2845,#2846,#1635,.T.);
#3565=EDGE_CURVE('',#2843,#2846,#1636,.T.);
#3566=EDGE_CURVE('',#2844,#2847,#1637,.T.);
#3567=EDGE_CURVE('',#2847,#2848,#1638,.T.);
#3568=EDGE_CURVE('',#2848,#2845,#1639,.T.);
#3569=EDGE_CURVE('',#2847,#2849,#1640,.T.);
#3570=EDGE_CURVE('',#2849,#2850,#1641,.T.);
#3571=EDGE_CURVE('',#2850,#2848,#1642,.T.);
#3572=EDGE_CURVE('',#2849,#2851,#1643,.T.);
#3573=EDGE_CURVE('',#2851,#2852,#1644,.T.);
#3574=EDGE_CURVE('',#2852,#2850,#1645,.T.);
#3575=EDGE_CURVE('',#2851,#2853,#1646,.T.);
#3576=EDGE_CURVE('',#2853,#2854,#1647,.T.);
#3577=EDGE_CURVE('',#2854,#2852,#1648,.T.);
#3578=EDGE_CURVE('',#2853,#2843,#1649,.T.);
#3579=EDGE_CURVE('',#2846,#2854,#1650,.T.);
#3580=EDGE_CURVE('',#2855,#2856,#1651,.T.);
#3581=EDGE_CURVE('',#2857,#2855,#1652,.T.);
#3582=EDGE_CURVE('',#2858,#2857,#1653,.T.);
#3583=EDGE_CURVE('',#2859,#2858,#1654,.T.);
#3584=EDGE_CURVE('',#2860,#2859,#1655,.T.);
#3585=EDGE_CURVE('',#2861,#2860,#1656,.T.);
#3586=EDGE_CURVE('',#2862,#2861,#1657,.T.);
#3587=EDGE_CURVE('',#2856,#2862,#1658,.T.);
#3588=EDGE_CURVE('',#2859,#2863,#1659,.T.);
#3589=EDGE_CURVE('',#2863,#2864,#1660,.T.);
#3590=EDGE_CURVE('',#2864,#2860,#1661,.T.);
#3591=EDGE_CURVE('',#2865,#2858,#1662,.T.);
#3592=EDGE_CURVE('',#2865,#2863,#1663,.T.);
#3593=EDGE_CURVE('',#2857,#2866,#1664,.T.);
#3594=EDGE_CURVE('',#2866,#2865,#1665,.T.);
#3595=EDGE_CURVE('',#2867,#2855,#1666,.T.);
#3596=EDGE_CURVE('',#2867,#2866,#1667,.T.);
#3597=EDGE_CURVE('',#2868,#2869,#1668,.T.);
#3598=EDGE_CURVE('',#2864,#2868,#1669,.T.);
#3599=EDGE_CURVE('',#2870,#2867,#1670,.T.);
#3600=EDGE_CURVE('',#2869,#2870,#1671,.T.);
#3601=EDGE_CURVE('',#2861,#2868,#1672,.T.);
#3602=EDGE_CURVE('',#2856,#2870,#1673,.T.);
#3603=EDGE_CURVE('',#2869,#2862,#1674,.T.);
#3604=EDGE_CURVE('',#2871,#2872,#1675,.T.);
#3605=EDGE_CURVE('',#2871,#2873,#1676,.T.);
#3606=EDGE_CURVE('',#2873,#2874,#1677,.T.);
#3607=EDGE_CURVE('',#2872,#2874,#1678,.T.);
#3608=EDGE_CURVE('',#2875,#2871,#1679,.T.);
#3609=EDGE_CURVE('',#2875,#2876,#1680,.T.);
#3610=EDGE_CURVE('',#2876,#2873,#1681,.T.);
#3611=EDGE_CURVE('',#2877,#2875,#1682,.T.);
#3612=EDGE_CURVE('',#2877,#2878,#1683,.T.);
#3613=EDGE_CURVE('',#2878,#2876,#1684,.T.);
#3614=EDGE_CURVE('',#2879,#2877,#1685,.T.);
#3615=EDGE_CURVE('',#2879,#2880,#1686,.T.);
#3616=EDGE_CURVE('',#2880,#2878,#1687,.T.);
#3617=EDGE_CURVE('',#2881,#2879,#1688,.T.);
#3618=EDGE_CURVE('',#2881,#2882,#1689,.T.);
#3619=EDGE_CURVE('',#2882,#2880,#1690,.T.);
#3620=EDGE_CURVE('',#2872,#2881,#1691,.T.);
#3621=EDGE_CURVE('',#2874,#2882,#1692,.T.);
#3622=EDGE_CURVE('',#2883,#2883,#2380,.T.);
#3623=EDGE_CURVE('',#2884,#2884,#2381,.T.);
#3624=EDGE_CURVE('',#2884,#2883,#1693,.T.);
#3625=EDGE_CURVE('',#2885,#2885,#2382,.F.);
#3626=EDGE_CURVE('',#2885,#2884,#1694,.T.);
#3627=EDGE_CURVE('',#2886,#2886,#2383,.T.);
#3628=EDGE_CURVE('',#2886,#2885,#1695,.T.);
#3629=ORIENTED_EDGE('',*,*,#2887,.F.);
#3630=ORIENTED_EDGE('',*,*,#2888,.T.);
#3631=ORIENTED_EDGE('',*,*,#2889,.F.);
#3632=ORIENTED_EDGE('',*,*,#2888,.F.);
#3633=ORIENTED_EDGE('',*,*,#2890,.F.);
#3634=ORIENTED_EDGE('',*,*,#2891,.T.);
#3635=ORIENTED_EDGE('',*,*,#2892,.F.);
#3636=ORIENTED_EDGE('',*,*,#2891,.F.);
#3637=ORIENTED_EDGE('',*,*,#2893,.F.);
#3638=ORIENTED_EDGE('',*,*,#2894,.T.);
#3639=ORIENTED_EDGE('',*,*,#2895,.F.);
#3640=ORIENTED_EDGE('',*,*,#2894,.F.);
#3641=ORIENTED_EDGE('',*,*,#2896,.F.);
#3642=ORIENTED_EDGE('',*,*,#2897,.T.);
#3643=ORIENTED_EDGE('',*,*,#2898,.F.);
#3644=ORIENTED_EDGE('',*,*,#2897,.F.);
#3645=ORIENTED_EDGE('',*,*,#2899,.T.);
#3646=ORIENTED_EDGE('',*,*,#2900,.T.);
#3647=ORIENTED_EDGE('',*,*,#2901,.F.);
#3648=ORIENTED_EDGE('',*,*,#2902,.F.);
#3649=ORIENTED_EDGE('',*,*,#2903,.T.);
#3650=ORIENTED_EDGE('',*,*,#2902,.T.);
#3651=ORIENTED_EDGE('',*,*,#2904,.F.);
#3652=ORIENTED_EDGE('',*,*,#2905,.F.);
#3653=ORIENTED_EDGE('',*,*,#2906,.T.);
#3654=ORIENTED_EDGE('',*,*,#2905,.T.);
#3655=ORIENTED_EDGE('',*,*,#2907,.F.);
#3656=ORIENTED_EDGE('',*,*,#2908,.F.);
#3657=ORIENTED_EDGE('',*,*,#2909,.T.);
#3658=ORIENTED_EDGE('',*,*,#2908,.T.);
#3659=ORIENTED_EDGE('',*,*,#2910,.F.);
#3660=ORIENTED_EDGE('',*,*,#2900,.F.);
#3661=ORIENTED_EDGE('',*,*,#2910,.T.);
#3662=ORIENTED_EDGE('',*,*,#2907,.T.);
#3663=ORIENTED_EDGE('',*,*,#2904,.T.);
#3664=ORIENTED_EDGE('',*,*,#2901,.T.);
#3665=ORIENTED_EDGE('',*,*,#2889,.T.);
#3666=ORIENTED_EDGE('',*,*,#2892,.T.);
#3667=ORIENTED_EDGE('',*,*,#2895,.T.);
#3668=ORIENTED_EDGE('',*,*,#2898,.T.);
#3669=ORIENTED_EDGE('',*,*,#2909,.F.);
#3670=ORIENTED_EDGE('',*,*,#2899,.F.);
#3671=ORIENTED_EDGE('',*,*,#2903,.F.);
#3672=ORIENTED_EDGE('',*,*,#2906,.F.);
#3673=ORIENTED_EDGE('',*,*,#2887,.T.);
#3674=ORIENTED_EDGE('',*,*,#2890,.T.);
#3675=ORIENTED_EDGE('',*,*,#2893,.T.);
#3676=ORIENTED_EDGE('',*,*,#2896,.T.);
#3677=ORIENTED_EDGE('',*,*,#2911,.T.);
#3678=ORIENTED_EDGE('',*,*,#2912,.T.);
#3679=ORIENTED_EDGE('',*,*,#2913,.F.);
#3680=ORIENTED_EDGE('',*,*,#2914,.F.);
#3681=ORIENTED_EDGE('',*,*,#2915,.T.);
#3682=ORIENTED_EDGE('',*,*,#2914,.T.);
#3683=ORIENTED_EDGE('',*,*,#2916,.F.);
#3684=ORIENTED_EDGE('',*,*,#2917,.F.);
#3685=ORIENTED_EDGE('',*,*,#2918,.T.);
#3686=ORIENTED_EDGE('',*,*,#2917,.T.);
#3687=ORIENTED_EDGE('',*,*,#2919,.F.);
#3688=ORIENTED_EDGE('',*,*,#2920,.F.);
#3689=ORIENTED_EDGE('',*,*,#2921,.T.);
#3690=ORIENTED_EDGE('',*,*,#2920,.T.);
#3691=ORIENTED_EDGE('',*,*,#2922,.F.);
#3692=ORIENTED_EDGE('',*,*,#2912,.F.);
#3693=ORIENTED_EDGE('',*,*,#2922,.T.);
#3694=ORIENTED_EDGE('',*,*,#2919,.T.);
#3695=ORIENTED_EDGE('',*,*,#2916,.T.);
#3696=ORIENTED_EDGE('',*,*,#2913,.T.);
#3697=ORIENTED_EDGE('',*,*,#2921,.F.);
#3698=ORIENTED_EDGE('',*,*,#2911,.F.);
#3699=ORIENTED_EDGE('',*,*,#2915,.F.);
#3700=ORIENTED_EDGE('',*,*,#2918,.F.);
#3701=ORIENTED_EDGE('',*,*,#2923,.T.);
#3702=ORIENTED_EDGE('',*,*,#2924,.T.);
#3703=ORIENTED_EDGE('',*,*,#2925,.F.);
#3704=ORIENTED_EDGE('',*,*,#2926,.F.);
#3705=ORIENTED_EDGE('',*,*,#2927,.T.);
#3706=ORIENTED_EDGE('',*,*,#2926,.T.);
#3707=ORIENTED_EDGE('',*,*,#2928,.F.);
#3708=ORIENTED_EDGE('',*,*,#2929,.F.);
#3709=ORIENTED_EDGE('',*,*,#2930,.T.);
#3710=ORIENTED_EDGE('',*,*,#2929,.T.);
#3711=ORIENTED_EDGE('',*,*,#2931,.F.);
#3712=ORIENTED_EDGE('',*,*,#2932,.F.);
#3713=ORIENTED_EDGE('',*,*,#2933,.T.);
#3714=ORIENTED_EDGE('',*,*,#2932,.T.);
#3715=ORIENTED_EDGE('',*,*,#2934,.F.);
#3716=ORIENTED_EDGE('',*,*,#2924,.F.);
#3717=ORIENTED_EDGE('',*,*,#2934,.T.);
#3718=ORIENTED_EDGE('',*,*,#2931,.T.);
#3719=ORIENTED_EDGE('',*,*,#2928,.T.);
#3720=ORIENTED_EDGE('',*,*,#2925,.T.);
#3721=ORIENTED_EDGE('',*,*,#2933,.F.);
#3722=ORIENTED_EDGE('',*,*,#2923,.F.);
#3723=ORIENTED_EDGE('',*,*,#2927,.F.);
#3724=ORIENTED_EDGE('',*,*,#2930,.F.);
#3725=ORIENTED_EDGE('',*,*,#2935,.F.);
#3726=ORIENTED_EDGE('',*,*,#2936,.T.);
#3727=ORIENTED_EDGE('',*,*,#2937,.T.);
#3728=ORIENTED_EDGE('',*,*,#2936,.F.);
#3729=ORIENTED_EDGE('',*,*,#2938,.F.);
#3730=ORIENTED_EDGE('',*,*,#2939,.T.);
#3731=ORIENTED_EDGE('',*,*,#2940,.T.);
#3732=ORIENTED_EDGE('',*,*,#2939,.F.);
#3733=ORIENTED_EDGE('',*,*,#2938,.T.);
#3734=ORIENTED_EDGE('',*,*,#2935,.T.);
#3735=ORIENTED_EDGE('',*,*,#2940,.F.);
#3736=ORIENTED_EDGE('',*,*,#2937,.F.);
#3737=ORIENTED_EDGE('',*,*,#2941,.F.);
#3738=ORIENTED_EDGE('',*,*,#2942,.T.);
#3739=ORIENTED_EDGE('',*,*,#2943,.T.);
#3740=ORIENTED_EDGE('',*,*,#2942,.F.);
#3741=ORIENTED_EDGE('',*,*,#2944,.F.);
#3742=ORIENTED_EDGE('',*,*,#2945,.T.);
#3743=ORIENTED_EDGE('',*,*,#2946,.T.);
#3744=ORIENTED_EDGE('',*,*,#2945,.F.);
#3745=ORIENTED_EDGE('',*,*,#2944,.T.);
#3746=ORIENTED_EDGE('',*,*,#2941,.T.);
#3747=ORIENTED_EDGE('',*,*,#2946,.F.);
#3748=ORIENTED_EDGE('',*,*,#2943,.F.);
#3749=ORIENTED_EDGE('',*,*,#2947,.F.);
#3750=ORIENTED_EDGE('',*,*,#2948,.T.);
#3751=ORIENTED_EDGE('',*,*,#2949,.T.);
#3752=ORIENTED_EDGE('',*,*,#2948,.F.);
#3753=ORIENTED_EDGE('',*,*,#2950,.F.);
#3754=ORIENTED_EDGE('',*,*,#2951,.T.);
#3755=ORIENTED_EDGE('',*,*,#2952,.T.);
#3756=ORIENTED_EDGE('',*,*,#2951,.F.);
#3757=ORIENTED_EDGE('',*,*,#2950,.T.);
#3758=ORIENTED_EDGE('',*,*,#2947,.T.);
#3759=ORIENTED_EDGE('',*,*,#2952,.F.);
#3760=ORIENTED_EDGE('',*,*,#2949,.F.);
#3761=ORIENTED_EDGE('',*,*,#2953,.F.);
#3762=ORIENTED_EDGE('',*,*,#2954,.T.);
#3763=ORIENTED_EDGE('',*,*,#2955,.T.);
#3764=ORIENTED_EDGE('',*,*,#2954,.F.);
#3765=ORIENTED_EDGE('',*,*,#2956,.F.);
#3766=ORIENTED_EDGE('',*,*,#2957,.T.);
#3767=ORIENTED_EDGE('',*,*,#2958,.T.);
#3768=ORIENTED_EDGE('',*,*,#2957,.F.);
#3769=ORIENTED_EDGE('',*,*,#2956,.T.);
#3770=ORIENTED_EDGE('',*,*,#2953,.T.);
#3771=ORIENTED_EDGE('',*,*,#2958,.F.);
#3772=ORIENTED_EDGE('',*,*,#2955,.F.);
#3773=ORIENTED_EDGE('',*,*,#2959,.F.);
#3774=ORIENTED_EDGE('',*,*,#2960,.T.);
#3775=ORIENTED_EDGE('',*,*,#2961,.F.);
#3776=ORIENTED_EDGE('',*,*,#2960,.F.);
#3777=ORIENTED_EDGE('',*,*,#2962,.F.);
#3778=ORIENTED_EDGE('',*,*,#2963,.T.);
#3779=ORIENTED_EDGE('',*,*,#2964,.F.);
#3780=ORIENTED_EDGE('',*,*,#2963,.F.);
#3781=ORIENTED_EDGE('',*,*,#2965,.T.);
#3782=ORIENTED_EDGE('',*,*,#2965,.F.);
#3783=ORIENTED_EDGE('',*,*,#2962,.T.);
#3784=ORIENTED_EDGE('',*,*,#2961,.T.);
#3785=ORIENTED_EDGE('',*,*,#2966,.F.);
#3786=ORIENTED_EDGE('',*,*,#2967,.T.);
#3787=ORIENTED_EDGE('',*,*,#2968,.F.);
#3788=ORIENTED_EDGE('',*,*,#2969,.F.);
#3789=ORIENTED_EDGE('',*,*,#2970,.F.);
#3790=ORIENTED_EDGE('',*,*,#2971,.T.);
#3791=ORIENTED_EDGE('',*,*,#2972,.F.);
#3792=ORIENTED_EDGE('',*,*,#2973,.F.);
#3793=ORIENTED_EDGE('',*,*,#2974,.T.);
#3794=ORIENTED_EDGE('',*,*,#2975,.F.);
#3795=ORIENTED_EDGE('',*,*,#2974,.F.);
#3796=ORIENTED_EDGE('',*,*,#2976,.F.);
#3797=ORIENTED_EDGE('',*,*,#2967,.F.);
#3798=ORIENTED_EDGE('',*,*,#2977,.F.);
#3799=ORIENTED_EDGE('',*,*,#2978,.T.);
#3800=ORIENTED_EDGE('',*,*,#2979,.F.);
#3801=ORIENTED_EDGE('',*,*,#2980,.F.);
#3802=ORIENTED_EDGE('',*,*,#2971,.F.);
#3803=ORIENTED_EDGE('',*,*,#2981,.F.);
#3804=ORIENTED_EDGE('',*,*,#2978,.F.);
#3805=ORIENTED_EDGE('',*,*,#2982,.T.);
#3806=ORIENTED_EDGE('',*,*,#2983,.T.);
#3807=ORIENTED_EDGE('',*,*,#2984,.T.);
#3808=ORIENTED_EDGE('',*,*,#2985,.T.);
#3809=ORIENTED_EDGE('',*,*,#2986,.T.);
#3810=ORIENTED_EDGE('',*,*,#2987,.T.);
#3811=ORIENTED_EDGE('',*,*,#2969,.T.);
#3812=ORIENTED_EDGE('',*,*,#2980,.T.);
#3813=ORIENTED_EDGE('',*,*,#2977,.T.);
#3814=ORIENTED_EDGE('',*,*,#2988,.T.);
#3815=ORIENTED_EDGE('',*,*,#2989,.T.);
#3816=ORIENTED_EDGE('',*,*,#2990,.T.);
#3817=ORIENTED_EDGE('',*,*,#2972,.T.);
#3818=ORIENTED_EDGE('',*,*,#2975,.T.);
#3819=ORIENTED_EDGE('',*,*,#2966,.T.);
#3820=ORIENTED_EDGE('',*,*,#2991,.T.);
#3821=ORIENTED_EDGE('',*,*,#2992,.T.);
#3822=ORIENTED_EDGE('',*,*,#2993,.T.);
#3823=ORIENTED_EDGE('',*,*,#2970,.T.);
#3824=ORIENTED_EDGE('',*,*,#2993,.F.);
#3825=ORIENTED_EDGE('',*,*,#2994,.F.);
#3826=ORIENTED_EDGE('',*,*,#2991,.F.);
#3827=ORIENTED_EDGE('',*,*,#2968,.T.);
#3828=ORIENTED_EDGE('',*,*,#2976,.T.);
#3829=ORIENTED_EDGE('',*,*,#2973,.T.);
#3830=ORIENTED_EDGE('',*,*,#2990,.F.);
#3831=ORIENTED_EDGE('',*,*,#2995,.F.);
#3832=ORIENTED_EDGE('',*,*,#2988,.F.);
#3833=ORIENTED_EDGE('',*,*,#2979,.T.);
#3834=ORIENTED_EDGE('',*,*,#2981,.T.);
#3835=ORIENTED_EDGE('',*,*,#2989,.F.);
#3836=ORIENTED_EDGE('',*,*,#2995,.T.);
#3837=ORIENTED_EDGE('',*,*,#2959,.T.);
#3838=ORIENTED_EDGE('',*,*,#2992,.F.);
#3839=ORIENTED_EDGE('',*,*,#2994,.T.);
#3840=ORIENTED_EDGE('',*,*,#2964,.T.);
#3841=ORIENTED_EDGE('',*,*,#2996,.F.);
#3842=ORIENTED_EDGE('',*,*,#2997,.T.);
#3843=ORIENTED_EDGE('',*,*,#2998,.T.);
#3844=ORIENTED_EDGE('',*,*,#2999,.F.);
#3845=ORIENTED_EDGE('',*,*,#3000,.F.);
#3846=ORIENTED_EDGE('',*,*,#3001,.T.);
#3847=ORIENTED_EDGE('',*,*,#3002,.T.);
#3848=ORIENTED_EDGE('',*,*,#2997,.F.);
#3849=ORIENTED_EDGE('',*,*,#3003,.F.);
#3850=ORIENTED_EDGE('',*,*,#3004,.T.);
#3851=ORIENTED_EDGE('',*,*,#3005,.T.);
#3852=ORIENTED_EDGE('',*,*,#3001,.F.);
#3853=ORIENTED_EDGE('',*,*,#3006,.F.);
#3854=ORIENTED_EDGE('',*,*,#2999,.T.);
#3855=ORIENTED_EDGE('',*,*,#3007,.T.);
#3856=ORIENTED_EDGE('',*,*,#3004,.F.);
#3857=ORIENTED_EDGE('',*,*,#3007,.F.);
#3858=ORIENTED_EDGE('',*,*,#2998,.F.);
#3859=ORIENTED_EDGE('',*,*,#3002,.F.);
#3860=ORIENTED_EDGE('',*,*,#3005,.F.);
#3861=ORIENTED_EDGE('',*,*,#3008,.F.);
#3862=ORIENTED_EDGE('',*,*,#3009,.T.);
#3863=ORIENTED_EDGE('',*,*,#2987,.F.);
#3864=ORIENTED_EDGE('',*,*,#3009,.F.);
#3865=ORIENTED_EDGE('',*,*,#3010,.F.);
#3866=ORIENTED_EDGE('',*,*,#3011,.T.);
#3867=ORIENTED_EDGE('',*,*,#2986,.F.);
#3868=ORIENTED_EDGE('',*,*,#3011,.F.);
#3869=ORIENTED_EDGE('',*,*,#3012,.T.);
#3870=ORIENTED_EDGE('',*,*,#3013,.T.);
#3871=ORIENTED_EDGE('',*,*,#2985,.F.);
#3872=ORIENTED_EDGE('',*,*,#3014,.F.);
#3873=ORIENTED_EDGE('',*,*,#3015,.T.);
#3874=ORIENTED_EDGE('',*,*,#3014,.T.);
#3875=ORIENTED_EDGE('',*,*,#2984,.F.);
#3876=ORIENTED_EDGE('',*,*,#3016,.F.);
#3877=ORIENTED_EDGE('',*,*,#3017,.T.);
#3878=ORIENTED_EDGE('',*,*,#3016,.T.);
#3879=ORIENTED_EDGE('',*,*,#2983,.F.);
#3880=ORIENTED_EDGE('',*,*,#3018,.F.);
#3881=ORIENTED_EDGE('',*,*,#3019,.T.);
#3882=ORIENTED_EDGE('',*,*,#3018,.T.);
#3883=ORIENTED_EDGE('',*,*,#2982,.F.);
#3884=ORIENTED_EDGE('',*,*,#3013,.F.);
#3885=ORIENTED_EDGE('',*,*,#3019,.F.);
#3886=ORIENTED_EDGE('',*,*,#3012,.F.);
#3887=ORIENTED_EDGE('',*,*,#3015,.F.);
#3888=ORIENTED_EDGE('',*,*,#3017,.F.);
#3889=ORIENTED_EDGE('',*,*,#2996,.T.);
#3890=ORIENTED_EDGE('',*,*,#3006,.T.);
#3891=ORIENTED_EDGE('',*,*,#3003,.T.);
#3892=ORIENTED_EDGE('',*,*,#3000,.T.);
#3893=ORIENTED_EDGE('',*,*,#3008,.T.);
#3894=ORIENTED_EDGE('',*,*,#3010,.T.);
#3895=ORIENTED_EDGE('',*,*,#3020,.T.);
#3896=ORIENTED_EDGE('',*,*,#3021,.T.);
#3897=ORIENTED_EDGE('',*,*,#3022,.F.);
#3898=ORIENTED_EDGE('',*,*,#3021,.F.);
#3899=ORIENTED_EDGE('',*,*,#3023,.F.);
#3900=ORIENTED_EDGE('',*,*,#3022,.T.);
#3901=ORIENTED_EDGE('',*,*,#3024,.T.);
#3902=ORIENTED_EDGE('',*,*,#3024,.F.);
#3903=ORIENTED_EDGE('',*,*,#3023,.T.);
#3904=ORIENTED_EDGE('',*,*,#3025,.F.);
#3905=ORIENTED_EDGE('',*,*,#3025,.T.);
#3906=ORIENTED_EDGE('',*,*,#3020,.F.);
#3907=ORIENTED_EDGE('',*,*,#3026,.F.);
#3908=ORIENTED_EDGE('',*,*,#3027,.F.);
#3909=ORIENTED_EDGE('',*,*,#3028,.F.);
#3910=ORIENTED_EDGE('',*,*,#3029,.T.);
#3911=ORIENTED_EDGE('',*,*,#3030,.F.);
#3912=ORIENTED_EDGE('',*,*,#3029,.F.);
#3913=ORIENTED_EDGE('',*,*,#3031,.F.);
#3914=ORIENTED_EDGE('',*,*,#3032,.T.);
#3915=ORIENTED_EDGE('',*,*,#3033,.F.);
#3916=ORIENTED_EDGE('',*,*,#3034,.F.);
#3917=ORIENTED_EDGE('',*,*,#3035,.F.);
#3918=ORIENTED_EDGE('',*,*,#3032,.F.);
#3919=ORIENTED_EDGE('',*,*,#3036,.F.);
#3920=ORIENTED_EDGE('',*,*,#3037,.T.);
#3921=ORIENTED_EDGE('',*,*,#3038,.T.);
#3922=ORIENTED_EDGE('',*,*,#3037,.F.);
#3923=ORIENTED_EDGE('',*,*,#3027,.T.);
#3924=ORIENTED_EDGE('',*,*,#3026,.T.);
#3925=ORIENTED_EDGE('',*,*,#3028,.T.);
#3926=ORIENTED_EDGE('',*,*,#3034,.T.);
#3927=ORIENTED_EDGE('',*,*,#3033,.T.);
#3928=ORIENTED_EDGE('',*,*,#3035,.T.);
#3929=ORIENTED_EDGE('',*,*,#3039,.T.);
#3930=ORIENTED_EDGE('',*,*,#3040,.T.);
#3931=ORIENTED_EDGE('',*,*,#3041,.T.);
#3932=ORIENTED_EDGE('',*,*,#3042,.T.);
#3933=ORIENTED_EDGE('',*,*,#3043,.T.);
#3934=ORIENTED_EDGE('',*,*,#3044,.T.);
#3935=ORIENTED_EDGE('',*,*,#3045,.T.);
#3936=ORIENTED_EDGE('',*,*,#3046,.T.);
#3937=ORIENTED_EDGE('',*,*,#3047,.T.);
#3938=ORIENTED_EDGE('',*,*,#3048,.T.);
#3939=ORIENTED_EDGE('',*,*,#3049,.T.);
#3940=ORIENTED_EDGE('',*,*,#3050,.T.);
#3941=ORIENTED_EDGE('',*,*,#3040,.F.);
#3942=ORIENTED_EDGE('',*,*,#3039,.F.);
#3943=ORIENTED_EDGE('',*,*,#3041,.F.);
#3944=ORIENTED_EDGE('',*,*,#3051,.T.);
#3945=ORIENTED_EDGE('',*,*,#3052,.F.);
#3946=ORIENTED_EDGE('',*,*,#3051,.F.);
#3947=ORIENTED_EDGE('',*,*,#3053,.F.);
#3948=ORIENTED_EDGE('',*,*,#3054,.T.);
#3949=ORIENTED_EDGE('',*,*,#3043,.F.);
#3950=ORIENTED_EDGE('',*,*,#3042,.F.);
#3951=ORIENTED_EDGE('',*,*,#3044,.F.);
#3952=ORIENTED_EDGE('',*,*,#3054,.F.);
#3953=ORIENTED_EDGE('',*,*,#3046,.F.);
#3954=ORIENTED_EDGE('',*,*,#3045,.F.);
#3955=ORIENTED_EDGE('',*,*,#3047,.F.);
#3956=ORIENTED_EDGE('',*,*,#3055,.T.);
#3957=ORIENTED_EDGE('',*,*,#3056,.F.);
#3958=ORIENTED_EDGE('',*,*,#3055,.F.);
#3959=ORIENTED_EDGE('',*,*,#3057,.F.);
#3960=ORIENTED_EDGE('',*,*,#3058,.T.);
#3961=ORIENTED_EDGE('',*,*,#3049,.F.);
#3962=ORIENTED_EDGE('',*,*,#3048,.F.);
#3963=ORIENTED_EDGE('',*,*,#3050,.F.);
#3964=ORIENTED_EDGE('',*,*,#3058,.F.);
#3965=ORIENTED_EDGE('',*,*,#3038,.F.);
#3966=ORIENTED_EDGE('',*,*,#3059,.T.);
#3967=ORIENTED_EDGE('',*,*,#3060,.F.);
#3968=ORIENTED_EDGE('',*,*,#3036,.T.);
#3969=ORIENTED_EDGE('',*,*,#3061,.F.);
#3970=ORIENTED_EDGE('',*,*,#3062,.T.);
#3971=ORIENTED_EDGE('',*,*,#3060,.T.);
#3972=ORIENTED_EDGE('',*,*,#3062,.F.);
#3973=ORIENTED_EDGE('',*,*,#3061,.T.);
#3974=ORIENTED_EDGE('',*,*,#3063,.F.);
#3975=ORIENTED_EDGE('',*,*,#3063,.T.);
#3976=ORIENTED_EDGE('',*,*,#3064,.T.);
#3977=ORIENTED_EDGE('',*,*,#3059,.F.);
#3978=ORIENTED_EDGE('',*,*,#3064,.F.);
#3979=ORIENTED_EDGE('',*,*,#3031,.T.);
#3980=ORIENTED_EDGE('',*,*,#3030,.T.);
#3981=ORIENTED_EDGE('',*,*,#3053,.T.);
#3982=ORIENTED_EDGE('',*,*,#3052,.T.);
#3983=ORIENTED_EDGE('',*,*,#3057,.T.);
#3984=ORIENTED_EDGE('',*,*,#3056,.T.);
#3985=ORIENTED_EDGE('',*,*,#3065,.F.);
#3986=ORIENTED_EDGE('',*,*,#3066,.T.);
#3987=ORIENTED_EDGE('',*,*,#3067,.T.);
#3988=ORIENTED_EDGE('',*,*,#3066,.F.);
#3989=ORIENTED_EDGE('',*,*,#3068,.F.);
#3990=ORIENTED_EDGE('',*,*,#3069,.T.);
#3991=ORIENTED_EDGE('',*,*,#3070,.T.);
#3992=ORIENTED_EDGE('',*,*,#3069,.F.);
#3993=ORIENTED_EDGE('',*,*,#3068,.T.);
#3994=ORIENTED_EDGE('',*,*,#3065,.T.);
#3995=ORIENTED_EDGE('',*,*,#3070,.F.);
#3996=ORIENTED_EDGE('',*,*,#3067,.F.);
#3997=ORIENTED_EDGE('',*,*,#3071,.T.);
#3998=ORIENTED_EDGE('',*,*,#3072,.T.);
#3999=ORIENTED_EDGE('',*,*,#3073,.T.);
#4000=ORIENTED_EDGE('',*,*,#3074,.F.);
#4001=ORIENTED_EDGE('',*,*,#3075,.T.);
#4002=ORIENTED_EDGE('',*,*,#3076,.T.);
#4003=ORIENTED_EDGE('',*,*,#3077,.T.);
#4004=ORIENTED_EDGE('',*,*,#3072,.F.);
#4005=ORIENTED_EDGE('',*,*,#3078,.T.);
#4006=ORIENTED_EDGE('',*,*,#3079,.T.);
#4007=ORIENTED_EDGE('',*,*,#3080,.T.);
#4008=ORIENTED_EDGE('',*,*,#3076,.F.);
#4009=ORIENTED_EDGE('',*,*,#3081,.T.);
#4010=ORIENTED_EDGE('',*,*,#3082,.T.);
#4011=ORIENTED_EDGE('',*,*,#3083,.T.);
#4012=ORIENTED_EDGE('',*,*,#3079,.F.);
#4013=ORIENTED_EDGE('',*,*,#3084,.T.);
#4014=ORIENTED_EDGE('',*,*,#3085,.T.);
#4015=ORIENTED_EDGE('',*,*,#3086,.T.);
#4016=ORIENTED_EDGE('',*,*,#3082,.F.);
#4017=ORIENTED_EDGE('',*,*,#3087,.T.);
#4018=ORIENTED_EDGE('',*,*,#3074,.T.);
#4019=ORIENTED_EDGE('',*,*,#3088,.T.);
#4020=ORIENTED_EDGE('',*,*,#3085,.F.);
#4021=ORIENTED_EDGE('',*,*,#3087,.F.);
#4022=ORIENTED_EDGE('',*,*,#3084,.F.);
#4023=ORIENTED_EDGE('',*,*,#3081,.F.);
#4024=ORIENTED_EDGE('',*,*,#3078,.F.);
#4025=ORIENTED_EDGE('',*,*,#3075,.F.);
#4026=ORIENTED_EDGE('',*,*,#3071,.F.);
#4027=ORIENTED_EDGE('',*,*,#3088,.F.);
#4028=ORIENTED_EDGE('',*,*,#3073,.F.);
#4029=ORIENTED_EDGE('',*,*,#3077,.F.);
#4030=ORIENTED_EDGE('',*,*,#3080,.F.);
#4031=ORIENTED_EDGE('',*,*,#3083,.F.);
#4032=ORIENTED_EDGE('',*,*,#3086,.F.);
#4033=ORIENTED_EDGE('',*,*,#3089,.F.);
#4034=ORIENTED_EDGE('',*,*,#3090,.F.);
#4035=ORIENTED_EDGE('',*,*,#3091,.F.);
#4036=ORIENTED_EDGE('',*,*,#3092,.T.);
#4037=ORIENTED_EDGE('',*,*,#3090,.T.);
#4038=ORIENTED_EDGE('',*,*,#3092,.F.);
#4039=ORIENTED_EDGE('',*,*,#3093,.F.);
#4040=ORIENTED_EDGE('',*,*,#3094,.T.);
#4041=ORIENTED_EDGE('',*,*,#3091,.T.);
#4042=ORIENTED_EDGE('',*,*,#3094,.F.);
#4043=ORIENTED_EDGE('',*,*,#3095,.F.);
#4044=ORIENTED_EDGE('',*,*,#3096,.T.);
#4045=ORIENTED_EDGE('',*,*,#3093,.T.);
#4046=ORIENTED_EDGE('',*,*,#3096,.F.);
#4047=ORIENTED_EDGE('',*,*,#3095,.T.);
#4048=ORIENTED_EDGE('',*,*,#3097,.F.);
#4049=ORIENTED_EDGE('',*,*,#3098,.F.);
#4050=ORIENTED_EDGE('',*,*,#3099,.T.);
#4051=ORIENTED_EDGE('',*,*,#3097,.T.);
#4052=ORIENTED_EDGE('',*,*,#3099,.F.);
#4053=ORIENTED_EDGE('',*,*,#3089,.T.);
#4054=ORIENTED_EDGE('',*,*,#3100,.T.);
#4055=ORIENTED_EDGE('',*,*,#3098,.T.);
#4056=ORIENTED_EDGE('',*,*,#3100,.F.);
#4057=ORIENTED_EDGE('',*,*,#3101,.F.);
#4058=ORIENTED_EDGE('',*,*,#3102,.T.);
#4059=ORIENTED_EDGE('',*,*,#3103,.F.);
#4060=ORIENTED_EDGE('',*,*,#3104,.T.);
#4061=ORIENTED_EDGE('',*,*,#3105,.F.);
#4062=ORIENTED_EDGE('',*,*,#3104,.F.);
#4063=ORIENTED_EDGE('',*,*,#3106,.F.);
#4064=ORIENTED_EDGE('',*,*,#3107,.F.);
#4065=ORIENTED_EDGE('',*,*,#3108,.F.);
#4066=ORIENTED_EDGE('',*,*,#3107,.T.);
#4067=ORIENTED_EDGE('',*,*,#3109,.T.);
#4068=ORIENTED_EDGE('',*,*,#3110,.T.);
#4069=ORIENTED_EDGE('',*,*,#3106,.T.);
#4070=ORIENTED_EDGE('',*,*,#3103,.T.);
#4071=ORIENTED_EDGE('',*,*,#3111,.T.);
#4072=ORIENTED_EDGE('',*,*,#3109,.F.);
#4073=ORIENTED_EDGE('',*,*,#3112,.F.);
#4074=ORIENTED_EDGE('',*,*,#3110,.F.);
#4075=ORIENTED_EDGE('',*,*,#3111,.F.);
#4076=ORIENTED_EDGE('',*,*,#3102,.F.);
#4077=ORIENTED_EDGE('',*,*,#3113,.F.);
#4078=ORIENTED_EDGE('',*,*,#3114,.T.);
#4079=ORIENTED_EDGE('',*,*,#3115,.F.);
#4080=ORIENTED_EDGE('',*,*,#3114,.F.);
#4081=ORIENTED_EDGE('',*,*,#3113,.T.);
#4082=ORIENTED_EDGE('',*,*,#3116,.F.);
#4083=ORIENTED_EDGE('',*,*,#3117,.T.);
#4084=ORIENTED_EDGE('',*,*,#3118,.T.);
#4085=ORIENTED_EDGE('',*,*,#3117,.F.);
#4086=ORIENTED_EDGE('',*,*,#3118,.F.);
#4087=ORIENTED_EDGE('',*,*,#3119,.F.);
#4088=ORIENTED_EDGE('',*,*,#3120,.T.);
#4089=ORIENTED_EDGE('',*,*,#3121,.F.);
#4090=ORIENTED_EDGE('',*,*,#3122,.T.);
#4091=ORIENTED_EDGE('',*,*,#3123,.F.);
#4092=ORIENTED_EDGE('',*,*,#3122,.F.);
#4093=ORIENTED_EDGE('',*,*,#3124,.F.);
#4094=ORIENTED_EDGE('',*,*,#3125,.F.);
#4095=ORIENTED_EDGE('',*,*,#3126,.F.);
#4096=ORIENTED_EDGE('',*,*,#3125,.T.);
#4097=ORIENTED_EDGE('',*,*,#3127,.T.);
#4098=ORIENTED_EDGE('',*,*,#3128,.T.);
#4099=ORIENTED_EDGE('',*,*,#3124,.T.);
#4100=ORIENTED_EDGE('',*,*,#3121,.T.);
#4101=ORIENTED_EDGE('',*,*,#3129,.T.);
#4102=ORIENTED_EDGE('',*,*,#3127,.F.);
#4103=ORIENTED_EDGE('',*,*,#3130,.F.);
#4104=ORIENTED_EDGE('',*,*,#3128,.F.);
#4105=ORIENTED_EDGE('',*,*,#3129,.F.);
#4106=ORIENTED_EDGE('',*,*,#3120,.F.);
#4107=ORIENTED_EDGE('',*,*,#3131,.F.);
#4108=ORIENTED_EDGE('',*,*,#3132,.T.);
#4109=ORIENTED_EDGE('',*,*,#3133,.F.);
#4110=ORIENTED_EDGE('',*,*,#3134,.T.);
#4111=ORIENTED_EDGE('',*,*,#3135,.F.);
#4112=ORIENTED_EDGE('',*,*,#3134,.F.);
#4113=ORIENTED_EDGE('',*,*,#3136,.F.);
#4114=ORIENTED_EDGE('',*,*,#3137,.F.);
#4115=ORIENTED_EDGE('',*,*,#3138,.F.);
#4116=ORIENTED_EDGE('',*,*,#3137,.T.);
#4117=ORIENTED_EDGE('',*,*,#3139,.T.);
#4118=ORIENTED_EDGE('',*,*,#3140,.T.);
#4119=ORIENTED_EDGE('',*,*,#3136,.T.);
#4120=ORIENTED_EDGE('',*,*,#3133,.T.);
#4121=ORIENTED_EDGE('',*,*,#3141,.T.);
#4122=ORIENTED_EDGE('',*,*,#3139,.F.);
#4123=ORIENTED_EDGE('',*,*,#3142,.F.);
#4124=ORIENTED_EDGE('',*,*,#3140,.F.);
#4125=ORIENTED_EDGE('',*,*,#3141,.F.);
#4126=ORIENTED_EDGE('',*,*,#3132,.F.);
#4127=ORIENTED_EDGE('',*,*,#3143,.F.);
#4128=ORIENTED_EDGE('',*,*,#3144,.T.);
#4129=ORIENTED_EDGE('',*,*,#3145,.F.);
#4130=ORIENTED_EDGE('',*,*,#3144,.F.);
#4131=ORIENTED_EDGE('',*,*,#3126,.T.);
#4132=ORIENTED_EDGE('',*,*,#3130,.T.);
#4133=ORIENTED_EDGE('',*,*,#3119,.T.);
#4134=ORIENTED_EDGE('',*,*,#3123,.T.);
#4135=ORIENTED_EDGE('',*,*,#3143,.T.);
#4136=ORIENTED_EDGE('',*,*,#3115,.T.);
#4137=ORIENTED_EDGE('',*,*,#3146,.F.);
#4138=ORIENTED_EDGE('',*,*,#3147,.T.);
#4139=ORIENTED_EDGE('',*,*,#3148,.T.);
#4140=ORIENTED_EDGE('',*,*,#3147,.F.);
#4141=ORIENTED_EDGE('',*,*,#3138,.T.);
#4142=ORIENTED_EDGE('',*,*,#3142,.T.);
#4143=ORIENTED_EDGE('',*,*,#3131,.T.);
#4144=ORIENTED_EDGE('',*,*,#3135,.T.);
#4145=ORIENTED_EDGE('',*,*,#3148,.F.);
#4146=ORIENTED_EDGE('',*,*,#3116,.T.);
#4147=ORIENTED_EDGE('',*,*,#3149,.F.);
#4148=ORIENTED_EDGE('',*,*,#3150,.T.);
#4149=ORIENTED_EDGE('',*,*,#3151,.T.);
#4150=ORIENTED_EDGE('',*,*,#3150,.F.);
#4151=ORIENTED_EDGE('',*,*,#3108,.T.);
#4152=ORIENTED_EDGE('',*,*,#3112,.T.);
#4153=ORIENTED_EDGE('',*,*,#3101,.T.);
#4154=ORIENTED_EDGE('',*,*,#3105,.T.);
#4155=ORIENTED_EDGE('',*,*,#3149,.T.);
#4156=ORIENTED_EDGE('',*,*,#3145,.T.);
#4157=ORIENTED_EDGE('',*,*,#3151,.F.);
#4158=ORIENTED_EDGE('',*,*,#3146,.T.);
#4159=ORIENTED_EDGE('',*,*,#3152,.F.);
#4160=ORIENTED_EDGE('',*,*,#3153,.T.);
#4161=ORIENTED_EDGE('',*,*,#3154,.T.);
#4162=ORIENTED_EDGE('',*,*,#3153,.F.);
#4163=ORIENTED_EDGE('',*,*,#3155,.F.);
#4164=ORIENTED_EDGE('',*,*,#3156,.T.);
#4165=ORIENTED_EDGE('',*,*,#3157,.T.);
#4166=ORIENTED_EDGE('',*,*,#3156,.F.);
#4167=ORIENTED_EDGE('',*,*,#3155,.T.);
#4168=ORIENTED_EDGE('',*,*,#3152,.T.);
#4169=ORIENTED_EDGE('',*,*,#3157,.F.);
#4170=ORIENTED_EDGE('',*,*,#3154,.F.);
#4171=ORIENTED_EDGE('',*,*,#3158,.F.);
#4172=ORIENTED_EDGE('',*,*,#3159,.T.);
#4173=ORIENTED_EDGE('',*,*,#3160,.T.);
#4174=ORIENTED_EDGE('',*,*,#3159,.F.);
#4175=ORIENTED_EDGE('',*,*,#3161,.F.);
#4176=ORIENTED_EDGE('',*,*,#3162,.T.);
#4177=ORIENTED_EDGE('',*,*,#3163,.T.);
#4178=ORIENTED_EDGE('',*,*,#3162,.F.);
#4179=ORIENTED_EDGE('',*,*,#3161,.T.);
#4180=ORIENTED_EDGE('',*,*,#3158,.T.);
#4181=ORIENTED_EDGE('',*,*,#3163,.F.);
#4182=ORIENTED_EDGE('',*,*,#3160,.F.);
#4183=ORIENTED_EDGE('',*,*,#3164,.F.);
#4184=ORIENTED_EDGE('',*,*,#3165,.T.);
#4185=ORIENTED_EDGE('',*,*,#3166,.T.);
#4186=ORIENTED_EDGE('',*,*,#3165,.F.);
#4187=ORIENTED_EDGE('',*,*,#3167,.F.);
#4188=ORIENTED_EDGE('',*,*,#3168,.T.);
#4189=ORIENTED_EDGE('',*,*,#3169,.T.);
#4190=ORIENTED_EDGE('',*,*,#3168,.F.);
#4191=ORIENTED_EDGE('',*,*,#3167,.T.);
#4192=ORIENTED_EDGE('',*,*,#3164,.T.);
#4193=ORIENTED_EDGE('',*,*,#3169,.F.);
#4194=ORIENTED_EDGE('',*,*,#3166,.F.);
#4195=ORIENTED_EDGE('',*,*,#3170,.F.);
#4196=ORIENTED_EDGE('',*,*,#3171,.T.);
#4197=ORIENTED_EDGE('',*,*,#3172,.T.);
#4198=ORIENTED_EDGE('',*,*,#3171,.F.);
#4199=ORIENTED_EDGE('',*,*,#3173,.F.);
#4200=ORIENTED_EDGE('',*,*,#3174,.T.);
#4201=ORIENTED_EDGE('',*,*,#3175,.T.);
#4202=ORIENTED_EDGE('',*,*,#3174,.F.);
#4203=ORIENTED_EDGE('',*,*,#3173,.T.);
#4204=ORIENTED_EDGE('',*,*,#3170,.T.);
#4205=ORIENTED_EDGE('',*,*,#3175,.F.);
#4206=ORIENTED_EDGE('',*,*,#3172,.F.);
#4207=ORIENTED_EDGE('',*,*,#3176,.F.);
#4208=ORIENTED_EDGE('',*,*,#3177,.T.);
#4209=ORIENTED_EDGE('',*,*,#3178,.T.);
#4210=ORIENTED_EDGE('',*,*,#3177,.F.);
#4211=ORIENTED_EDGE('',*,*,#3179,.F.);
#4212=ORIENTED_EDGE('',*,*,#3180,.T.);
#4213=ORIENTED_EDGE('',*,*,#3181,.T.);
#4214=ORIENTED_EDGE('',*,*,#3180,.F.);
#4215=ORIENTED_EDGE('',*,*,#3179,.T.);
#4216=ORIENTED_EDGE('',*,*,#3176,.T.);
#4217=ORIENTED_EDGE('',*,*,#3181,.F.);
#4218=ORIENTED_EDGE('',*,*,#3178,.F.);
#4219=ORIENTED_EDGE('',*,*,#3182,.F.);
#4220=ORIENTED_EDGE('',*,*,#3183,.T.);
#4221=ORIENTED_EDGE('',*,*,#3184,.F.);
#4222=ORIENTED_EDGE('',*,*,#3185,.F.);
#4223=ORIENTED_EDGE('',*,*,#3186,.T.);
#4224=ORIENTED_EDGE('',*,*,#3187,.F.);
#4225=ORIENTED_EDGE('',*,*,#3188,.F.);
#4226=ORIENTED_EDGE('',*,*,#3186,.F.);
#4227=ORIENTED_EDGE('',*,*,#3189,.F.);
#4228=ORIENTED_EDGE('',*,*,#3190,.F.);
#4229=ORIENTED_EDGE('',*,*,#3183,.F.);
#4230=ORIENTED_EDGE('',*,*,#3191,.F.);
#4231=ORIENTED_EDGE('',*,*,#3189,.T.);
#4232=ORIENTED_EDGE('',*,*,#3185,.T.);
#4233=ORIENTED_EDGE('',*,*,#3192,.F.);
#4234=ORIENTED_EDGE('',*,*,#3193,.T.);
#4235=ORIENTED_EDGE('',*,*,#3194,.F.);
#4236=ORIENTED_EDGE('',*,*,#3195,.F.);
#4237=ORIENTED_EDGE('',*,*,#3196,.F.);
#4238=ORIENTED_EDGE('',*,*,#3197,.T.);
#4239=ORIENTED_EDGE('',*,*,#3198,.F.);
#4240=ORIENTED_EDGE('',*,*,#3193,.F.);
#4241=ORIENTED_EDGE('',*,*,#3199,.F.);
#4242=ORIENTED_EDGE('',*,*,#3200,.F.);
#4243=ORIENTED_EDGE('',*,*,#3201,.F.);
#4244=ORIENTED_EDGE('',*,*,#3197,.F.);
#4245=ORIENTED_EDGE('',*,*,#3202,.T.);
#4246=ORIENTED_EDGE('',*,*,#3194,.T.);
#4247=ORIENTED_EDGE('',*,*,#3198,.T.);
#4248=ORIENTED_EDGE('',*,*,#3201,.T.);
#4249=ORIENTED_EDGE('',*,*,#3203,.T.);
#4250=ORIENTED_EDGE('',*,*,#3195,.T.);
#4251=ORIENTED_EDGE('',*,*,#3203,.F.);
#4252=ORIENTED_EDGE('',*,*,#3200,.T.);
#4253=ORIENTED_EDGE('',*,*,#3204,.T.);
#4254=ORIENTED_EDGE('',*,*,#3190,.T.);
#4255=ORIENTED_EDGE('',*,*,#3191,.T.);
#4256=ORIENTED_EDGE('',*,*,#3184,.T.);
#4257=ORIENTED_EDGE('',*,*,#3182,.T.);
#4258=ORIENTED_EDGE('',*,*,#3202,.F.);
#4259=ORIENTED_EDGE('',*,*,#3205,.T.);
#4260=ORIENTED_EDGE('',*,*,#3206,.T.);
#4261=ORIENTED_EDGE('',*,*,#3205,.F.);
#4262=ORIENTED_EDGE('',*,*,#3187,.T.);
#4263=ORIENTED_EDGE('',*,*,#3188,.T.);
#4264=ORIENTED_EDGE('',*,*,#3206,.F.);
#4265=ORIENTED_EDGE('',*,*,#3192,.T.);
#4266=ORIENTED_EDGE('',*,*,#3204,.F.);
#4267=ORIENTED_EDGE('',*,*,#3199,.T.);
#4268=ORIENTED_EDGE('',*,*,#3196,.T.);
#4269=ORIENTED_EDGE('',*,*,#3207,.F.);
#4270=ORIENTED_EDGE('',*,*,#3208,.T.);
#4271=ORIENTED_EDGE('',*,*,#3209,.F.);
#4272=ORIENTED_EDGE('',*,*,#3210,.F.);
#4273=ORIENTED_EDGE('',*,*,#3211,.T.);
#4274=ORIENTED_EDGE('',*,*,#3212,.F.);
#4275=ORIENTED_EDGE('',*,*,#3213,.F.);
#4276=ORIENTED_EDGE('',*,*,#3211,.F.);
#4277=ORIENTED_EDGE('',*,*,#3214,.F.);
#4278=ORIENTED_EDGE('',*,*,#3215,.F.);
#4279=ORIENTED_EDGE('',*,*,#3208,.F.);
#4280=ORIENTED_EDGE('',*,*,#3216,.F.);
#4281=ORIENTED_EDGE('',*,*,#3214,.T.);
#4282=ORIENTED_EDGE('',*,*,#3210,.T.);
#4283=ORIENTED_EDGE('',*,*,#3217,.F.);
#4284=ORIENTED_EDGE('',*,*,#3218,.T.);
#4285=ORIENTED_EDGE('',*,*,#3219,.T.);
#4286=ORIENTED_EDGE('',*,*,#3218,.F.);
#4287=ORIENTED_EDGE('',*,*,#3215,.T.);
#4288=ORIENTED_EDGE('',*,*,#3216,.T.);
#4289=ORIENTED_EDGE('',*,*,#3209,.T.);
#4290=ORIENTED_EDGE('',*,*,#3207,.T.);
#4291=ORIENTED_EDGE('',*,*,#3220,.F.);
#4292=ORIENTED_EDGE('',*,*,#3221,.T.);
#4293=ORIENTED_EDGE('',*,*,#3222,.T.);
#4294=ORIENTED_EDGE('',*,*,#3221,.F.);
#4295=ORIENTED_EDGE('',*,*,#3212,.T.);
#4296=ORIENTED_EDGE('',*,*,#3213,.T.);
#4297=ORIENTED_EDGE('',*,*,#3220,.T.);
#4298=ORIENTED_EDGE('',*,*,#3217,.T.);
#4299=ORIENTED_EDGE('',*,*,#3222,.F.);
#4300=ORIENTED_EDGE('',*,*,#3219,.F.);
#4301=ORIENTED_EDGE('',*,*,#3223,.F.);
#4302=ORIENTED_EDGE('',*,*,#3224,.T.);
#4303=ORIENTED_EDGE('',*,*,#3225,.F.);
#4304=ORIENTED_EDGE('',*,*,#3226,.F.);
#4305=ORIENTED_EDGE('',*,*,#3227,.T.);
#4306=ORIENTED_EDGE('',*,*,#3228,.F.);
#4307=ORIENTED_EDGE('',*,*,#3229,.F.);
#4308=ORIENTED_EDGE('',*,*,#3227,.F.);
#4309=ORIENTED_EDGE('',*,*,#3230,.F.);
#4310=ORIENTED_EDGE('',*,*,#3231,.F.);
#4311=ORIENTED_EDGE('',*,*,#3224,.F.);
#4312=ORIENTED_EDGE('',*,*,#3232,.F.);
#4313=ORIENTED_EDGE('',*,*,#3230,.T.);
#4314=ORIENTED_EDGE('',*,*,#3226,.T.);
#4315=ORIENTED_EDGE('',*,*,#3233,.F.);
#4316=ORIENTED_EDGE('',*,*,#3234,.T.);
#4317=ORIENTED_EDGE('',*,*,#3235,.T.);
#4318=ORIENTED_EDGE('',*,*,#3234,.F.);
#4319=ORIENTED_EDGE('',*,*,#3231,.T.);
#4320=ORIENTED_EDGE('',*,*,#3232,.T.);
#4321=ORIENTED_EDGE('',*,*,#3225,.T.);
#4322=ORIENTED_EDGE('',*,*,#3223,.T.);
#4323=ORIENTED_EDGE('',*,*,#3236,.F.);
#4324=ORIENTED_EDGE('',*,*,#3237,.T.);
#4325=ORIENTED_EDGE('',*,*,#3238,.T.);
#4326=ORIENTED_EDGE('',*,*,#3237,.F.);
#4327=ORIENTED_EDGE('',*,*,#3228,.T.);
#4328=ORIENTED_EDGE('',*,*,#3229,.T.);
#4329=ORIENTED_EDGE('',*,*,#3236,.T.);
#4330=ORIENTED_EDGE('',*,*,#3233,.T.);
#4331=ORIENTED_EDGE('',*,*,#3238,.F.);
#4332=ORIENTED_EDGE('',*,*,#3235,.F.);
#4333=ORIENTED_EDGE('',*,*,#3239,.F.);
#4334=ORIENTED_EDGE('',*,*,#3240,.T.);
#4335=ORIENTED_EDGE('',*,*,#3241,.F.);
#4336=ORIENTED_EDGE('',*,*,#3242,.F.);
#4337=ORIENTED_EDGE('',*,*,#3243,.F.);
#4338=ORIENTED_EDGE('',*,*,#3244,.T.);
#4339=ORIENTED_EDGE('',*,*,#3245,.F.);
#4340=ORIENTED_EDGE('',*,*,#3240,.F.);
#4341=ORIENTED_EDGE('',*,*,#3246,.F.);
#4342=ORIENTED_EDGE('',*,*,#3247,.F.);
#4343=ORIENTED_EDGE('',*,*,#3248,.F.);
#4344=ORIENTED_EDGE('',*,*,#3249,.F.);
#4345=ORIENTED_EDGE('',*,*,#3244,.F.);
#4346=ORIENTED_EDGE('',*,*,#3250,.T.);
#4347=ORIENTED_EDGE('',*,*,#3241,.T.);
#4348=ORIENTED_EDGE('',*,*,#3245,.T.);
#4349=ORIENTED_EDGE('',*,*,#3249,.T.);
#4350=ORIENTED_EDGE('',*,*,#3251,.T.);
#4351=ORIENTED_EDGE('',*,*,#3242,.T.);
#4352=ORIENTED_EDGE('',*,*,#3251,.F.);
#4353=ORIENTED_EDGE('',*,*,#3248,.T.);
#4354=ORIENTED_EDGE('',*,*,#3252,.F.);
#4355=ORIENTED_EDGE('',*,*,#3253,.T.);
#4356=ORIENTED_EDGE('',*,*,#3254,.T.);
#4357=ORIENTED_EDGE('',*,*,#3255,.T.);
#4358=ORIENTED_EDGE('',*,*,#3256,.T.);
#4359=ORIENTED_EDGE('',*,*,#3257,.T.);
#4360=ORIENTED_EDGE('',*,*,#3258,.T.);
#4361=ORIENTED_EDGE('',*,*,#3259,.F.);
#4362=ORIENTED_EDGE('',*,*,#3260,.F.);
#4363=ORIENTED_EDGE('',*,*,#3261,.F.);
#4364=ORIENTED_EDGE('',*,*,#3262,.T.);
#4365=ORIENTED_EDGE('',*,*,#3255,.F.);
#4366=ORIENTED_EDGE('',*,*,#3256,.F.);
#4367=ORIENTED_EDGE('',*,*,#3262,.F.);
#4368=ORIENTED_EDGE('',*,*,#3257,.F.);
#4369=ORIENTED_EDGE('',*,*,#3258,.F.);
#4370=ORIENTED_EDGE('',*,*,#3263,.T.);
#4371=ORIENTED_EDGE('',*,*,#3264,.F.);
#4372=ORIENTED_EDGE('',*,*,#3265,.F.);
#4373=ORIENTED_EDGE('',*,*,#3266,.F.);
#4374=ORIENTED_EDGE('',*,*,#3263,.F.);
#4375=ORIENTED_EDGE('',*,*,#3267,.F.);
#4376=ORIENTED_EDGE('',*,*,#3268,.T.);
#4377=ORIENTED_EDGE('',*,*,#3260,.T.);
#4378=ORIENTED_EDGE('',*,*,#3269,.T.);
#4379=ORIENTED_EDGE('',*,*,#3270,.F.);
#4380=ORIENTED_EDGE('',*,*,#3269,.F.);
#4381=ORIENTED_EDGE('',*,*,#3259,.T.);
#4382=ORIENTED_EDGE('',*,*,#3261,.T.);
#4383=ORIENTED_EDGE('',*,*,#3268,.F.);
#4384=ORIENTED_EDGE('',*,*,#3265,.T.);
#4385=ORIENTED_EDGE('',*,*,#3264,.T.);
#4386=ORIENTED_EDGE('',*,*,#3266,.T.);
#4387=ORIENTED_EDGE('',*,*,#3271,.T.);
#4388=ORIENTED_EDGE('',*,*,#3272,.T.);
#4389=ORIENTED_EDGE('',*,*,#3273,.T.);
#4390=ORIENTED_EDGE('',*,*,#3274,.T.);
#4391=ORIENTED_EDGE('',*,*,#3275,.T.);
#4392=ORIENTED_EDGE('',*,*,#3276,.T.);
#4393=ORIENTED_EDGE('',*,*,#3272,.F.);
#4394=ORIENTED_EDGE('',*,*,#3271,.F.);
#4395=ORIENTED_EDGE('',*,*,#3273,.F.);
#4396=ORIENTED_EDGE('',*,*,#3277,.T.);
#4397=ORIENTED_EDGE('',*,*,#3246,.T.);
#4398=ORIENTED_EDGE('',*,*,#3277,.F.);
#4399=ORIENTED_EDGE('',*,*,#3253,.F.);
#4400=ORIENTED_EDGE('',*,*,#3254,.F.);
#4401=ORIENTED_EDGE('',*,*,#3278,.T.);
#4402=ORIENTED_EDGE('',*,*,#3275,.F.);
#4403=ORIENTED_EDGE('',*,*,#3274,.F.);
#4404=ORIENTED_EDGE('',*,*,#3276,.F.);
#4405=ORIENTED_EDGE('',*,*,#3278,.F.);
#4406=ORIENTED_EDGE('',*,*,#3267,.T.);
#4407=ORIENTED_EDGE('',*,*,#3239,.T.);
#4408=ORIENTED_EDGE('',*,*,#3252,.T.);
#4409=ORIENTED_EDGE('',*,*,#3247,.T.);
#4410=ORIENTED_EDGE('',*,*,#3243,.T.);
#4411=ORIENTED_EDGE('',*,*,#3279,.T.);
#4412=ORIENTED_EDGE('',*,*,#3280,.T.);
#4413=ORIENTED_EDGE('',*,*,#3281,.F.);
#4414=ORIENTED_EDGE('',*,*,#3282,.T.);
#4415=ORIENTED_EDGE('',*,*,#3283,.F.);
#4416=ORIENTED_EDGE('',*,*,#3284,.T.);
#4417=ORIENTED_EDGE('',*,*,#3285,.F.);
#4418=ORIENTED_EDGE('',*,*,#3286,.T.);
#4419=ORIENTED_EDGE('',*,*,#3287,.F.);
#4420=ORIENTED_EDGE('',*,*,#3288,.T.);
#4421=ORIENTED_EDGE('',*,*,#3289,.F.);
#4422=ORIENTED_EDGE('',*,*,#3290,.T.);
#4423=ORIENTED_EDGE('',*,*,#3291,.F.);
#4424=ORIENTED_EDGE('',*,*,#3292,.T.);
#4425=ORIENTED_EDGE('',*,*,#3293,.F.);
#4426=ORIENTED_EDGE('',*,*,#3294,.T.);
#4427=ORIENTED_EDGE('',*,*,#3295,.F.);
#4428=ORIENTED_EDGE('',*,*,#3296,.T.);
#4429=ORIENTED_EDGE('',*,*,#3297,.F.);
#4430=ORIENTED_EDGE('',*,*,#3298,.T.);
#4431=ORIENTED_EDGE('',*,*,#3299,.F.);
#4432=ORIENTED_EDGE('',*,*,#3300,.T.);
#4433=ORIENTED_EDGE('',*,*,#3301,.F.);
#4434=ORIENTED_EDGE('',*,*,#3302,.T.);
#4435=ORIENTED_EDGE('',*,*,#3303,.F.);
#4436=ORIENTED_EDGE('',*,*,#3304,.T.);
#4437=ORIENTED_EDGE('',*,*,#3305,.F.);
#4438=ORIENTED_EDGE('',*,*,#3306,.T.);
#4439=ORIENTED_EDGE('',*,*,#3307,.F.);
#4440=ORIENTED_EDGE('',*,*,#3308,.T.);
#4441=ORIENTED_EDGE('',*,*,#3309,.F.);
#4442=ORIENTED_EDGE('',*,*,#3310,.T.);
#4443=ORIENTED_EDGE('',*,*,#3311,.F.);
#4444=ORIENTED_EDGE('',*,*,#3312,.T.);
#4445=ORIENTED_EDGE('',*,*,#3313,.F.);
#4446=ORIENTED_EDGE('',*,*,#3314,.T.);
#4447=ORIENTED_EDGE('',*,*,#3315,.F.);
#4448=ORIENTED_EDGE('',*,*,#3316,.T.);
#4449=ORIENTED_EDGE('',*,*,#3317,.F.);
#4450=ORIENTED_EDGE('',*,*,#3318,.T.);
#4451=ORIENTED_EDGE('',*,*,#3319,.F.);
#4452=ORIENTED_EDGE('',*,*,#3320,.T.);
#4453=ORIENTED_EDGE('',*,*,#3321,.F.);
#4454=ORIENTED_EDGE('',*,*,#3322,.T.);
#4455=ORIENTED_EDGE('',*,*,#3323,.F.);
#4456=ORIENTED_EDGE('',*,*,#3324,.T.);
#4457=ORIENTED_EDGE('',*,*,#3325,.F.);
#4458=ORIENTED_EDGE('',*,*,#3326,.T.);
#4459=ORIENTED_EDGE('',*,*,#3327,.F.);
#4460=ORIENTED_EDGE('',*,*,#3328,.T.);
#4461=ORIENTED_EDGE('',*,*,#3329,.F.);
#4462=ORIENTED_EDGE('',*,*,#3330,.T.);
#4463=ORIENTED_EDGE('',*,*,#3331,.F.);
#4464=ORIENTED_EDGE('',*,*,#3332,.T.);
#4465=ORIENTED_EDGE('',*,*,#3333,.F.);
#4466=ORIENTED_EDGE('',*,*,#3334,.T.);
#4467=ORIENTED_EDGE('',*,*,#3335,.F.);
#4468=ORIENTED_EDGE('',*,*,#3336,.T.);
#4469=ORIENTED_EDGE('',*,*,#3337,.F.);
#4470=ORIENTED_EDGE('',*,*,#3338,.T.);
#4471=ORIENTED_EDGE('',*,*,#3339,.F.);
#4472=ORIENTED_EDGE('',*,*,#3340,.T.);
#4473=ORIENTED_EDGE('',*,*,#3341,.F.);
#4474=ORIENTED_EDGE('',*,*,#3342,.T.);
#4475=ORIENTED_EDGE('',*,*,#3343,.F.);
#4476=ORIENTED_EDGE('',*,*,#3344,.T.);
#4477=ORIENTED_EDGE('',*,*,#3345,.F.);
#4478=ORIENTED_EDGE('',*,*,#3346,.T.);
#4479=ORIENTED_EDGE('',*,*,#3347,.F.);
#4480=ORIENTED_EDGE('',*,*,#3348,.T.);
#4481=ORIENTED_EDGE('',*,*,#3349,.F.);
#4482=ORIENTED_EDGE('',*,*,#3350,.T.);
#4483=ORIENTED_EDGE('',*,*,#3351,.F.);
#4484=ORIENTED_EDGE('',*,*,#3352,.T.);
#4485=ORIENTED_EDGE('',*,*,#3353,.F.);
#4486=ORIENTED_EDGE('',*,*,#3354,.T.);
#4487=ORIENTED_EDGE('',*,*,#3355,.F.);
#4488=ORIENTED_EDGE('',*,*,#3356,.T.);
#4489=ORIENTED_EDGE('',*,*,#3357,.F.);
#4490=ORIENTED_EDGE('',*,*,#3358,.T.);
#4491=ORIENTED_EDGE('',*,*,#3359,.F.);
#4492=ORIENTED_EDGE('',*,*,#3360,.F.);
#4493=ORIENTED_EDGE('',*,*,#3361,.T.);
#4494=ORIENTED_EDGE('',*,*,#3279,.F.);
#4495=ORIENTED_EDGE('',*,*,#3361,.F.);
#4496=ORIENTED_EDGE('',*,*,#3360,.T.);
#4497=ORIENTED_EDGE('',*,*,#3270,.T.);
#4498=ORIENTED_EDGE('',*,*,#3362,.F.);
#4499=ORIENTED_EDGE('',*,*,#3363,.T.);
#4500=ORIENTED_EDGE('',*,*,#3364,.T.);
#4501=ORIENTED_EDGE('',*,*,#3365,.T.);
#4502=ORIENTED_EDGE('',*,*,#3366,.T.);
#4503=ORIENTED_EDGE('',*,*,#3367,.T.);
#4504=ORIENTED_EDGE('',*,*,#3368,.T.);
#4505=ORIENTED_EDGE('',*,*,#3369,.T.);
#4506=ORIENTED_EDGE('',*,*,#3370,.T.);
#4507=ORIENTED_EDGE('',*,*,#3371,.T.);
#4508=ORIENTED_EDGE('',*,*,#3372,.T.);
#4509=ORIENTED_EDGE('',*,*,#3373,.T.);
#4510=ORIENTED_EDGE('',*,*,#3374,.T.);
#4511=ORIENTED_EDGE('',*,*,#3375,.T.);
#4512=ORIENTED_EDGE('',*,*,#3376,.T.);
#4513=ORIENTED_EDGE('',*,*,#3377,.T.);
#4514=ORIENTED_EDGE('',*,*,#3378,.T.);
#4515=ORIENTED_EDGE('',*,*,#3379,.T.);
#4516=ORIENTED_EDGE('',*,*,#3380,.T.);
#4517=ORIENTED_EDGE('',*,*,#3381,.T.);
#4518=ORIENTED_EDGE('',*,*,#3382,.T.);
#4519=ORIENTED_EDGE('',*,*,#3383,.T.);
#4520=ORIENTED_EDGE('',*,*,#3384,.T.);
#4521=ORIENTED_EDGE('',*,*,#3385,.T.);
#4522=ORIENTED_EDGE('',*,*,#3386,.T.);
#4523=ORIENTED_EDGE('',*,*,#3387,.T.);
#4524=ORIENTED_EDGE('',*,*,#3388,.T.);
#4525=ORIENTED_EDGE('',*,*,#3389,.T.);
#4526=ORIENTED_EDGE('',*,*,#3390,.T.);
#4527=ORIENTED_EDGE('',*,*,#3391,.T.);
#4528=ORIENTED_EDGE('',*,*,#3392,.T.);
#4529=ORIENTED_EDGE('',*,*,#3393,.T.);
#4530=ORIENTED_EDGE('',*,*,#3394,.T.);
#4531=ORIENTED_EDGE('',*,*,#3395,.T.);
#4532=ORIENTED_EDGE('',*,*,#3396,.T.);
#4533=ORIENTED_EDGE('',*,*,#3397,.T.);
#4534=ORIENTED_EDGE('',*,*,#3398,.T.);
#4535=ORIENTED_EDGE('',*,*,#3399,.T.);
#4536=ORIENTED_EDGE('',*,*,#3400,.T.);
#4537=ORIENTED_EDGE('',*,*,#3401,.T.);
#4538=ORIENTED_EDGE('',*,*,#3402,.T.);
#4539=ORIENTED_EDGE('',*,*,#3403,.T.);
#4540=ORIENTED_EDGE('',*,*,#3404,.T.);
#4541=ORIENTED_EDGE('',*,*,#3405,.T.);
#4542=ORIENTED_EDGE('',*,*,#3406,.T.);
#4543=ORIENTED_EDGE('',*,*,#3407,.T.);
#4544=ORIENTED_EDGE('',*,*,#3408,.T.);
#4545=ORIENTED_EDGE('',*,*,#3409,.T.);
#4546=ORIENTED_EDGE('',*,*,#3410,.T.);
#4547=ORIENTED_EDGE('',*,*,#3411,.T.);
#4548=ORIENTED_EDGE('',*,*,#3412,.T.);
#4549=ORIENTED_EDGE('',*,*,#3413,.T.);
#4550=ORIENTED_EDGE('',*,*,#3414,.T.);
#4551=ORIENTED_EDGE('',*,*,#3415,.T.);
#4552=ORIENTED_EDGE('',*,*,#3416,.T.);
#4553=ORIENTED_EDGE('',*,*,#3417,.T.);
#4554=ORIENTED_EDGE('',*,*,#3418,.T.);
#4555=ORIENTED_EDGE('',*,*,#3419,.T.);
#4556=ORIENTED_EDGE('',*,*,#3420,.T.);
#4557=ORIENTED_EDGE('',*,*,#3421,.T.);
#4558=ORIENTED_EDGE('',*,*,#3422,.T.);
#4559=ORIENTED_EDGE('',*,*,#3423,.T.);
#4560=ORIENTED_EDGE('',*,*,#3424,.T.);
#4561=ORIENTED_EDGE('',*,*,#3425,.T.);
#4562=ORIENTED_EDGE('',*,*,#3426,.T.);
#4563=ORIENTED_EDGE('',*,*,#3427,.T.);
#4564=ORIENTED_EDGE('',*,*,#3428,.T.);
#4565=ORIENTED_EDGE('',*,*,#3429,.T.);
#4566=ORIENTED_EDGE('',*,*,#3430,.T.);
#4567=ORIENTED_EDGE('',*,*,#3431,.T.);
#4568=ORIENTED_EDGE('',*,*,#3432,.T.);
#4569=ORIENTED_EDGE('',*,*,#3433,.T.);
#4570=ORIENTED_EDGE('',*,*,#3434,.T.);
#4571=ORIENTED_EDGE('',*,*,#3435,.T.);
#4572=ORIENTED_EDGE('',*,*,#3436,.T.);
#4573=ORIENTED_EDGE('',*,*,#3437,.T.);
#4574=ORIENTED_EDGE('',*,*,#3438,.T.);
#4575=ORIENTED_EDGE('',*,*,#3439,.T.);
#4576=ORIENTED_EDGE('',*,*,#3440,.T.);
#4577=ORIENTED_EDGE('',*,*,#3441,.T.);
#4578=ORIENTED_EDGE('',*,*,#3442,.T.);
#4579=ORIENTED_EDGE('',*,*,#3250,.F.);
#4580=ORIENTED_EDGE('',*,*,#3443,.T.);
#4581=ORIENTED_EDGE('',*,*,#3362,.T.);
#4582=ORIENTED_EDGE('',*,*,#3443,.F.);
#4583=ORIENTED_EDGE('',*,*,#3444,.F.);
#4584=ORIENTED_EDGE('',*,*,#3363,.F.);
#4585=ORIENTED_EDGE('',*,*,#3445,.F.);
#4586=ORIENTED_EDGE('',*,*,#3280,.F.);
#4587=ORIENTED_EDGE('',*,*,#3445,.T.);
#4588=ORIENTED_EDGE('',*,*,#3442,.F.);
#4589=ORIENTED_EDGE('',*,*,#3446,.T.);
#4590=ORIENTED_EDGE('',*,*,#3281,.T.);
#4591=ORIENTED_EDGE('',*,*,#3446,.F.);
#4592=ORIENTED_EDGE('',*,*,#3441,.F.);
#4593=ORIENTED_EDGE('',*,*,#3447,.F.);
#4594=ORIENTED_EDGE('',*,*,#3282,.F.);
#4595=ORIENTED_EDGE('',*,*,#3447,.T.);
#4596=ORIENTED_EDGE('',*,*,#3440,.F.);
#4597=ORIENTED_EDGE('',*,*,#3448,.T.);
#4598=ORIENTED_EDGE('',*,*,#3283,.T.);
#4599=ORIENTED_EDGE('',*,*,#3448,.F.);
#4600=ORIENTED_EDGE('',*,*,#3439,.F.);
#4601=ORIENTED_EDGE('',*,*,#3449,.F.);
#4602=ORIENTED_EDGE('',*,*,#3284,.F.);
#4603=ORIENTED_EDGE('',*,*,#3449,.T.);
#4604=ORIENTED_EDGE('',*,*,#3438,.F.);
#4605=ORIENTED_EDGE('',*,*,#3450,.T.);
#4606=ORIENTED_EDGE('',*,*,#3285,.T.);
#4607=ORIENTED_EDGE('',*,*,#3450,.F.);
#4608=ORIENTED_EDGE('',*,*,#3437,.F.);
#4609=ORIENTED_EDGE('',*,*,#3451,.F.);
#4610=ORIENTED_EDGE('',*,*,#3286,.F.);
#4611=ORIENTED_EDGE('',*,*,#3451,.T.);
#4612=ORIENTED_EDGE('',*,*,#3436,.F.);
#4613=ORIENTED_EDGE('',*,*,#3452,.T.);
#4614=ORIENTED_EDGE('',*,*,#3287,.T.);
#4615=ORIENTED_EDGE('',*,*,#3452,.F.);
#4616=ORIENTED_EDGE('',*,*,#3435,.F.);
#4617=ORIENTED_EDGE('',*,*,#3453,.F.);
#4618=ORIENTED_EDGE('',*,*,#3288,.F.);
#4619=ORIENTED_EDGE('',*,*,#3453,.T.);
#4620=ORIENTED_EDGE('',*,*,#3434,.F.);
#4621=ORIENTED_EDGE('',*,*,#3454,.T.);
#4622=ORIENTED_EDGE('',*,*,#3289,.T.);
#4623=ORIENTED_EDGE('',*,*,#3454,.F.);
#4624=ORIENTED_EDGE('',*,*,#3433,.F.);
#4625=ORIENTED_EDGE('',*,*,#3455,.F.);
#4626=ORIENTED_EDGE('',*,*,#3290,.F.);
#4627=ORIENTED_EDGE('',*,*,#3455,.T.);
#4628=ORIENTED_EDGE('',*,*,#3432,.F.);
#4629=ORIENTED_EDGE('',*,*,#3456,.T.);
#4630=ORIENTED_EDGE('',*,*,#3291,.T.);
#4631=ORIENTED_EDGE('',*,*,#3456,.F.);
#4632=ORIENTED_EDGE('',*,*,#3431,.F.);
#4633=ORIENTED_EDGE('',*,*,#3457,.F.);
#4634=ORIENTED_EDGE('',*,*,#3292,.F.);
#4635=ORIENTED_EDGE('',*,*,#3457,.T.);
#4636=ORIENTED_EDGE('',*,*,#3430,.F.);
#4637=ORIENTED_EDGE('',*,*,#3458,.T.);
#4638=ORIENTED_EDGE('',*,*,#3293,.T.);
#4639=ORIENTED_EDGE('',*,*,#3458,.F.);
#4640=ORIENTED_EDGE('',*,*,#3429,.F.);
#4641=ORIENTED_EDGE('',*,*,#3459,.F.);
#4642=ORIENTED_EDGE('',*,*,#3294,.F.);
#4643=ORIENTED_EDGE('',*,*,#3459,.T.);
#4644=ORIENTED_EDGE('',*,*,#3428,.F.);
#4645=ORIENTED_EDGE('',*,*,#3460,.T.);
#4646=ORIENTED_EDGE('',*,*,#3295,.T.);
#4647=ORIENTED_EDGE('',*,*,#3460,.F.);
#4648=ORIENTED_EDGE('',*,*,#3427,.F.);
#4649=ORIENTED_EDGE('',*,*,#3461,.F.);
#4650=ORIENTED_EDGE('',*,*,#3296,.F.);
#4651=ORIENTED_EDGE('',*,*,#3461,.T.);
#4652=ORIENTED_EDGE('',*,*,#3426,.F.);
#4653=ORIENTED_EDGE('',*,*,#3462,.T.);
#4654=ORIENTED_EDGE('',*,*,#3297,.T.);
#4655=ORIENTED_EDGE('',*,*,#3462,.F.);
#4656=ORIENTED_EDGE('',*,*,#3425,.F.);
#4657=ORIENTED_EDGE('',*,*,#3463,.F.);
#4658=ORIENTED_EDGE('',*,*,#3298,.F.);
#4659=ORIENTED_EDGE('',*,*,#3463,.T.);
#4660=ORIENTED_EDGE('',*,*,#3424,.F.);
#4661=ORIENTED_EDGE('',*,*,#3464,.T.);
#4662=ORIENTED_EDGE('',*,*,#3299,.T.);
#4663=ORIENTED_EDGE('',*,*,#3464,.F.);
#4664=ORIENTED_EDGE('',*,*,#3423,.F.);
#4665=ORIENTED_EDGE('',*,*,#3465,.F.);
#4666=ORIENTED_EDGE('',*,*,#3300,.F.);
#4667=ORIENTED_EDGE('',*,*,#3465,.T.);
#4668=ORIENTED_EDGE('',*,*,#3422,.F.);
#4669=ORIENTED_EDGE('',*,*,#3466,.T.);
#4670=ORIENTED_EDGE('',*,*,#3301,.T.);
#4671=ORIENTED_EDGE('',*,*,#3466,.F.);
#4672=ORIENTED_EDGE('',*,*,#3421,.F.);
#4673=ORIENTED_EDGE('',*,*,#3467,.F.);
#4674=ORIENTED_EDGE('',*,*,#3302,.F.);
#4675=ORIENTED_EDGE('',*,*,#3467,.T.);
#4676=ORIENTED_EDGE('',*,*,#3420,.F.);
#4677=ORIENTED_EDGE('',*,*,#3468,.T.);
#4678=ORIENTED_EDGE('',*,*,#3303,.T.);
#4679=ORIENTED_EDGE('',*,*,#3468,.F.);
#4680=ORIENTED_EDGE('',*,*,#3419,.F.);
#4681=ORIENTED_EDGE('',*,*,#3469,.F.);
#4682=ORIENTED_EDGE('',*,*,#3304,.F.);
#4683=ORIENTED_EDGE('',*,*,#3469,.T.);
#4684=ORIENTED_EDGE('',*,*,#3418,.F.);
#4685=ORIENTED_EDGE('',*,*,#3470,.T.);
#4686=ORIENTED_EDGE('',*,*,#3305,.T.);
#4687=ORIENTED_EDGE('',*,*,#3470,.F.);
#4688=ORIENTED_EDGE('',*,*,#3417,.F.);
#4689=ORIENTED_EDGE('',*,*,#3471,.F.);
#4690=ORIENTED_EDGE('',*,*,#3306,.F.);
#4691=ORIENTED_EDGE('',*,*,#3471,.T.);
#4692=ORIENTED_EDGE('',*,*,#3416,.F.);
#4693=ORIENTED_EDGE('',*,*,#3472,.T.);
#4694=ORIENTED_EDGE('',*,*,#3307,.T.);
#4695=ORIENTED_EDGE('',*,*,#3472,.F.);
#4696=ORIENTED_EDGE('',*,*,#3415,.F.);
#4697=ORIENTED_EDGE('',*,*,#3473,.F.);
#4698=ORIENTED_EDGE('',*,*,#3308,.F.);
#4699=ORIENTED_EDGE('',*,*,#3473,.T.);
#4700=ORIENTED_EDGE('',*,*,#3414,.F.);
#4701=ORIENTED_EDGE('',*,*,#3474,.T.);
#4702=ORIENTED_EDGE('',*,*,#3309,.T.);
#4703=ORIENTED_EDGE('',*,*,#3474,.F.);
#4704=ORIENTED_EDGE('',*,*,#3413,.F.);
#4705=ORIENTED_EDGE('',*,*,#3475,.F.);
#4706=ORIENTED_EDGE('',*,*,#3310,.F.);
#4707=ORIENTED_EDGE('',*,*,#3475,.T.);
#4708=ORIENTED_EDGE('',*,*,#3412,.F.);
#4709=ORIENTED_EDGE('',*,*,#3476,.T.);
#4710=ORIENTED_EDGE('',*,*,#3311,.T.);
#4711=ORIENTED_EDGE('',*,*,#3476,.F.);
#4712=ORIENTED_EDGE('',*,*,#3411,.F.);
#4713=ORIENTED_EDGE('',*,*,#3477,.F.);
#4714=ORIENTED_EDGE('',*,*,#3312,.F.);
#4715=ORIENTED_EDGE('',*,*,#3477,.T.);
#4716=ORIENTED_EDGE('',*,*,#3410,.F.);
#4717=ORIENTED_EDGE('',*,*,#3478,.T.);
#4718=ORIENTED_EDGE('',*,*,#3313,.T.);
#4719=ORIENTED_EDGE('',*,*,#3478,.F.);
#4720=ORIENTED_EDGE('',*,*,#3409,.F.);
#4721=ORIENTED_EDGE('',*,*,#3479,.F.);
#4722=ORIENTED_EDGE('',*,*,#3314,.F.);
#4723=ORIENTED_EDGE('',*,*,#3479,.T.);
#4724=ORIENTED_EDGE('',*,*,#3408,.F.);
#4725=ORIENTED_EDGE('',*,*,#3480,.T.);
#4726=ORIENTED_EDGE('',*,*,#3315,.T.);
#4727=ORIENTED_EDGE('',*,*,#3480,.F.);
#4728=ORIENTED_EDGE('',*,*,#3407,.F.);
#4729=ORIENTED_EDGE('',*,*,#3481,.F.);
#4730=ORIENTED_EDGE('',*,*,#3316,.F.);
#4731=ORIENTED_EDGE('',*,*,#3481,.T.);
#4732=ORIENTED_EDGE('',*,*,#3406,.F.);
#4733=ORIENTED_EDGE('',*,*,#3482,.T.);
#4734=ORIENTED_EDGE('',*,*,#3317,.T.);
#4735=ORIENTED_EDGE('',*,*,#3482,.F.);
#4736=ORIENTED_EDGE('',*,*,#3405,.F.);
#4737=ORIENTED_EDGE('',*,*,#3483,.F.);
#4738=ORIENTED_EDGE('',*,*,#3318,.F.);
#4739=ORIENTED_EDGE('',*,*,#3483,.T.);
#4740=ORIENTED_EDGE('',*,*,#3404,.F.);
#4741=ORIENTED_EDGE('',*,*,#3484,.T.);
#4742=ORIENTED_EDGE('',*,*,#3319,.T.);
#4743=ORIENTED_EDGE('',*,*,#3484,.F.);
#4744=ORIENTED_EDGE('',*,*,#3403,.F.);
#4745=ORIENTED_EDGE('',*,*,#3485,.F.);
#4746=ORIENTED_EDGE('',*,*,#3320,.F.);
#4747=ORIENTED_EDGE('',*,*,#3485,.T.);
#4748=ORIENTED_EDGE('',*,*,#3402,.F.);
#4749=ORIENTED_EDGE('',*,*,#3486,.T.);
#4750=ORIENTED_EDGE('',*,*,#3321,.T.);
#4751=ORIENTED_EDGE('',*,*,#3486,.F.);
#4752=ORIENTED_EDGE('',*,*,#3401,.F.);
#4753=ORIENTED_EDGE('',*,*,#3487,.F.);
#4754=ORIENTED_EDGE('',*,*,#3322,.F.);
#4755=ORIENTED_EDGE('',*,*,#3487,.T.);
#4756=ORIENTED_EDGE('',*,*,#3400,.F.);
#4757=ORIENTED_EDGE('',*,*,#3488,.T.);
#4758=ORIENTED_EDGE('',*,*,#3323,.T.);
#4759=ORIENTED_EDGE('',*,*,#3488,.F.);
#4760=ORIENTED_EDGE('',*,*,#3399,.F.);
#4761=ORIENTED_EDGE('',*,*,#3489,.F.);
#4762=ORIENTED_EDGE('',*,*,#3324,.F.);
#4763=ORIENTED_EDGE('',*,*,#3489,.T.);
#4764=ORIENTED_EDGE('',*,*,#3398,.F.);
#4765=ORIENTED_EDGE('',*,*,#3490,.T.);
#4766=ORIENTED_EDGE('',*,*,#3325,.T.);
#4767=ORIENTED_EDGE('',*,*,#3490,.F.);
#4768=ORIENTED_EDGE('',*,*,#3397,.F.);
#4769=ORIENTED_EDGE('',*,*,#3491,.F.);
#4770=ORIENTED_EDGE('',*,*,#3326,.F.);
#4771=ORIENTED_EDGE('',*,*,#3491,.T.);
#4772=ORIENTED_EDGE('',*,*,#3396,.F.);
#4773=ORIENTED_EDGE('',*,*,#3492,.T.);
#4774=ORIENTED_EDGE('',*,*,#3327,.T.);
#4775=ORIENTED_EDGE('',*,*,#3492,.F.);
#4776=ORIENTED_EDGE('',*,*,#3395,.F.);
#4777=ORIENTED_EDGE('',*,*,#3493,.F.);
#4778=ORIENTED_EDGE('',*,*,#3328,.F.);
#4779=ORIENTED_EDGE('',*,*,#3493,.T.);
#4780=ORIENTED_EDGE('',*,*,#3394,.F.);
#4781=ORIENTED_EDGE('',*,*,#3494,.T.);
#4782=ORIENTED_EDGE('',*,*,#3329,.T.);
#4783=ORIENTED_EDGE('',*,*,#3494,.F.);
#4784=ORIENTED_EDGE('',*,*,#3393,.F.);
#4785=ORIENTED_EDGE('',*,*,#3495,.F.);
#4786=ORIENTED_EDGE('',*,*,#3330,.F.);
#4787=ORIENTED_EDGE('',*,*,#3495,.T.);
#4788=ORIENTED_EDGE('',*,*,#3392,.F.);
#4789=ORIENTED_EDGE('',*,*,#3496,.T.);
#4790=ORIENTED_EDGE('',*,*,#3331,.T.);
#4791=ORIENTED_EDGE('',*,*,#3496,.F.);
#4792=ORIENTED_EDGE('',*,*,#3391,.F.);
#4793=ORIENTED_EDGE('',*,*,#3497,.F.);
#4794=ORIENTED_EDGE('',*,*,#3332,.F.);
#4795=ORIENTED_EDGE('',*,*,#3497,.T.);
#4796=ORIENTED_EDGE('',*,*,#3390,.F.);
#4797=ORIENTED_EDGE('',*,*,#3498,.T.);
#4798=ORIENTED_EDGE('',*,*,#3333,.T.);
#4799=ORIENTED_EDGE('',*,*,#3498,.F.);
#4800=ORIENTED_EDGE('',*,*,#3389,.F.);
#4801=ORIENTED_EDGE('',*,*,#3499,.F.);
#4802=ORIENTED_EDGE('',*,*,#3334,.F.);
#4803=ORIENTED_EDGE('',*,*,#3499,.T.);
#4804=ORIENTED_EDGE('',*,*,#3388,.F.);
#4805=ORIENTED_EDGE('',*,*,#3500,.T.);
#4806=ORIENTED_EDGE('',*,*,#3335,.T.);
#4807=ORIENTED_EDGE('',*,*,#3500,.F.);
#4808=ORIENTED_EDGE('',*,*,#3387,.F.);
#4809=ORIENTED_EDGE('',*,*,#3501,.F.);
#4810=ORIENTED_EDGE('',*,*,#3336,.F.);
#4811=ORIENTED_EDGE('',*,*,#3501,.T.);
#4812=ORIENTED_EDGE('',*,*,#3386,.F.);
#4813=ORIENTED_EDGE('',*,*,#3502,.T.);
#4814=ORIENTED_EDGE('',*,*,#3337,.T.);
#4815=ORIENTED_EDGE('',*,*,#3502,.F.);
#4816=ORIENTED_EDGE('',*,*,#3385,.F.);
#4817=ORIENTED_EDGE('',*,*,#3503,.F.);
#4818=ORIENTED_EDGE('',*,*,#3338,.F.);
#4819=ORIENTED_EDGE('',*,*,#3503,.T.);
#4820=ORIENTED_EDGE('',*,*,#3384,.F.);
#4821=ORIENTED_EDGE('',*,*,#3504,.T.);
#4822=ORIENTED_EDGE('',*,*,#3339,.T.);
#4823=ORIENTED_EDGE('',*,*,#3504,.F.);
#4824=ORIENTED_EDGE('',*,*,#3383,.F.);
#4825=ORIENTED_EDGE('',*,*,#3505,.F.);
#4826=ORIENTED_EDGE('',*,*,#3340,.F.);
#4827=ORIENTED_EDGE('',*,*,#3505,.T.);
#4828=ORIENTED_EDGE('',*,*,#3382,.F.);
#4829=ORIENTED_EDGE('',*,*,#3506,.T.);
#4830=ORIENTED_EDGE('',*,*,#3341,.T.);
#4831=ORIENTED_EDGE('',*,*,#3506,.F.);
#4832=ORIENTED_EDGE('',*,*,#3381,.F.);
#4833=ORIENTED_EDGE('',*,*,#3507,.F.);
#4834=ORIENTED_EDGE('',*,*,#3342,.F.);
#4835=ORIENTED_EDGE('',*,*,#3507,.T.);
#4836=ORIENTED_EDGE('',*,*,#3380,.F.);
#4837=ORIENTED_EDGE('',*,*,#3508,.T.);
#4838=ORIENTED_EDGE('',*,*,#3343,.T.);
#4839=ORIENTED_EDGE('',*,*,#3508,.F.);
#4840=ORIENTED_EDGE('',*,*,#3379,.F.);
#4841=ORIENTED_EDGE('',*,*,#3509,.F.);
#4842=ORIENTED_EDGE('',*,*,#3344,.F.);
#4843=ORIENTED_EDGE('',*,*,#3509,.T.);
#4844=ORIENTED_EDGE('',*,*,#3378,.F.);
#4845=ORIENTED_EDGE('',*,*,#3510,.T.);
#4846=ORIENTED_EDGE('',*,*,#3345,.T.);
#4847=ORIENTED_EDGE('',*,*,#3510,.F.);
#4848=ORIENTED_EDGE('',*,*,#3377,.F.);
#4849=ORIENTED_EDGE('',*,*,#3511,.F.);
#4850=ORIENTED_EDGE('',*,*,#3346,.F.);
#4851=ORIENTED_EDGE('',*,*,#3511,.T.);
#4852=ORIENTED_EDGE('',*,*,#3376,.F.);
#4853=ORIENTED_EDGE('',*,*,#3512,.T.);
#4854=ORIENTED_EDGE('',*,*,#3347,.T.);
#4855=ORIENTED_EDGE('',*,*,#3512,.F.);
#4856=ORIENTED_EDGE('',*,*,#3375,.F.);
#4857=ORIENTED_EDGE('',*,*,#3513,.F.);
#4858=ORIENTED_EDGE('',*,*,#3348,.F.);
#4859=ORIENTED_EDGE('',*,*,#3513,.T.);
#4860=ORIENTED_EDGE('',*,*,#3374,.F.);
#4861=ORIENTED_EDGE('',*,*,#3514,.T.);
#4862=ORIENTED_EDGE('',*,*,#3349,.T.);
#4863=ORIENTED_EDGE('',*,*,#3514,.F.);
#4864=ORIENTED_EDGE('',*,*,#3373,.F.);
#4865=ORIENTED_EDGE('',*,*,#3515,.F.);
#4866=ORIENTED_EDGE('',*,*,#3350,.F.);
#4867=ORIENTED_EDGE('',*,*,#3515,.T.);
#4868=ORIENTED_EDGE('',*,*,#3372,.F.);
#4869=ORIENTED_EDGE('',*,*,#3516,.T.);
#4870=ORIENTED_EDGE('',*,*,#3351,.T.);
#4871=ORIENTED_EDGE('',*,*,#3516,.F.);
#4872=ORIENTED_EDGE('',*,*,#3371,.F.);
#4873=ORIENTED_EDGE('',*,*,#3517,.F.);
#4874=ORIENTED_EDGE('',*,*,#3352,.F.);
#4875=ORIENTED_EDGE('',*,*,#3517,.T.);
#4876=ORIENTED_EDGE('',*,*,#3370,.F.);
#4877=ORIENTED_EDGE('',*,*,#3518,.T.);
#4878=ORIENTED_EDGE('',*,*,#3353,.T.);
#4879=ORIENTED_EDGE('',*,*,#3518,.F.);
#4880=ORIENTED_EDGE('',*,*,#3369,.F.);
#4881=ORIENTED_EDGE('',*,*,#3519,.F.);
#4882=ORIENTED_EDGE('',*,*,#3354,.F.);
#4883=ORIENTED_EDGE('',*,*,#3519,.T.);
#4884=ORIENTED_EDGE('',*,*,#3368,.F.);
#4885=ORIENTED_EDGE('',*,*,#3520,.T.);
#4886=ORIENTED_EDGE('',*,*,#3355,.T.);
#4887=ORIENTED_EDGE('',*,*,#3521,.F.);
#4888=ORIENTED_EDGE('',*,*,#3356,.F.);
#4889=ORIENTED_EDGE('',*,*,#3520,.F.);
#4890=ORIENTED_EDGE('',*,*,#3367,.F.);
#4891=ORIENTED_EDGE('',*,*,#3444,.T.);
#4892=ORIENTED_EDGE('',*,*,#3359,.T.);
#4893=ORIENTED_EDGE('',*,*,#3522,.T.);
#4894=ORIENTED_EDGE('',*,*,#3364,.F.);
#4895=ORIENTED_EDGE('',*,*,#3523,.F.);
#4896=ORIENTED_EDGE('',*,*,#3365,.F.);
#4897=ORIENTED_EDGE('',*,*,#3522,.F.);
#4898=ORIENTED_EDGE('',*,*,#3358,.F.);
#4899=ORIENTED_EDGE('',*,*,#3521,.T.);
#4900=ORIENTED_EDGE('',*,*,#3366,.F.);
#4901=ORIENTED_EDGE('',*,*,#3523,.T.);
#4902=ORIENTED_EDGE('',*,*,#3357,.T.);
#4903=ORIENTED_EDGE('',*,*,#3524,.F.);
#4904=ORIENTED_EDGE('',*,*,#3525,.F.);
#4905=ORIENTED_EDGE('',*,*,#3526,.F.);
#4906=ORIENTED_EDGE('',*,*,#3527,.F.);
#4907=ORIENTED_EDGE('',*,*,#3528,.F.);
#4908=ORIENTED_EDGE('',*,*,#3529,.F.);
#4909=ORIENTED_EDGE('',*,*,#3530,.F.);
#4910=ORIENTED_EDGE('',*,*,#3531,.F.);
#4911=ORIENTED_EDGE('',*,*,#3528,.T.);
#4912=ORIENTED_EDGE('',*,*,#3532,.T.);
#4913=ORIENTED_EDGE('',*,*,#3533,.T.);
#4914=ORIENTED_EDGE('',*,*,#3534,.T.);
#4915=ORIENTED_EDGE('',*,*,#3527,.T.);
#4916=ORIENTED_EDGE('',*,*,#3535,.F.);
#4917=ORIENTED_EDGE('',*,*,#3536,.T.);
#4918=ORIENTED_EDGE('',*,*,#3532,.F.);
#4919=ORIENTED_EDGE('',*,*,#3526,.T.);
#4920=ORIENTED_EDGE('',*,*,#3537,.T.);
#4921=ORIENTED_EDGE('',*,*,#3538,.T.);
#4922=ORIENTED_EDGE('',*,*,#3535,.T.);
#4923=ORIENTED_EDGE('',*,*,#3525,.T.);
#4924=ORIENTED_EDGE('',*,*,#3539,.F.);
#4925=ORIENTED_EDGE('',*,*,#3540,.T.);
#4926=ORIENTED_EDGE('',*,*,#3537,.F.);
#4927=ORIENTED_EDGE('',*,*,#3533,.F.);
#4928=ORIENTED_EDGE('',*,*,#3536,.F.);
#4929=ORIENTED_EDGE('',*,*,#3538,.F.);
#4930=ORIENTED_EDGE('',*,*,#3540,.F.);
#4931=ORIENTED_EDGE('',*,*,#3541,.F.);
#4932=ORIENTED_EDGE('',*,*,#3542,.F.);
#4933=ORIENTED_EDGE('',*,*,#3543,.F.);
#4934=ORIENTED_EDGE('',*,*,#3544,.F.);
#4935=ORIENTED_EDGE('',*,*,#3524,.T.);
#4936=ORIENTED_EDGE('',*,*,#3545,.T.);
#4937=ORIENTED_EDGE('',*,*,#3541,.T.);
#4938=ORIENTED_EDGE('',*,*,#3539,.T.);
#4939=ORIENTED_EDGE('',*,*,#3531,.T.);
#4940=ORIENTED_EDGE('',*,*,#3546,.F.);
#4941=ORIENTED_EDGE('',*,*,#3542,.T.);
#4942=ORIENTED_EDGE('',*,*,#3545,.F.);
#4943=ORIENTED_EDGE('',*,*,#3530,.T.);
#4944=ORIENTED_EDGE('',*,*,#3547,.T.);
#4945=ORIENTED_EDGE('',*,*,#3543,.T.);
#4946=ORIENTED_EDGE('',*,*,#3546,.T.);
#4947=ORIENTED_EDGE('',*,*,#3529,.T.);
#4948=ORIENTED_EDGE('',*,*,#3534,.F.);
#4949=ORIENTED_EDGE('',*,*,#3544,.T.);
#4950=ORIENTED_EDGE('',*,*,#3547,.F.);
#4951=ORIENTED_EDGE('',*,*,#3548,.F.);
#4952=ORIENTED_EDGE('',*,*,#3549,.F.);
#4953=ORIENTED_EDGE('',*,*,#3550,.T.);
#4954=ORIENTED_EDGE('',*,*,#3548,.T.);
#4955=ORIENTED_EDGE('',*,*,#3550,.F.);
#4956=ORIENTED_EDGE('',*,*,#3551,.F.);
#4957=ORIENTED_EDGE('',*,*,#3552,.T.);
#4958=ORIENTED_EDGE('',*,*,#3549,.T.);
#4959=ORIENTED_EDGE('',*,*,#3552,.F.);
#4960=ORIENTED_EDGE('',*,*,#3553,.F.);
#4961=ORIENTED_EDGE('',*,*,#3554,.T.);
#4962=ORIENTED_EDGE('',*,*,#3551,.T.);
#4963=ORIENTED_EDGE('',*,*,#3554,.F.);
#4964=ORIENTED_EDGE('',*,*,#3553,.T.);
#4965=ORIENTED_EDGE('',*,*,#3555,.F.);
#4966=ORIENTED_EDGE('',*,*,#3556,.F.);
#4967=ORIENTED_EDGE('',*,*,#3557,.T.);
#4968=ORIENTED_EDGE('',*,*,#3555,.T.);
#4969=ORIENTED_EDGE('',*,*,#3557,.F.);
#4970=ORIENTED_EDGE('',*,*,#3558,.F.);
#4971=ORIENTED_EDGE('',*,*,#3559,.T.);
#4972=ORIENTED_EDGE('',*,*,#3556,.T.);
#4973=ORIENTED_EDGE('',*,*,#3559,.F.);
#4974=ORIENTED_EDGE('',*,*,#3560,.F.);
#4975=ORIENTED_EDGE('',*,*,#3561,.T.);
#4976=ORIENTED_EDGE('',*,*,#3558,.T.);
#4977=ORIENTED_EDGE('',*,*,#3561,.F.);
#4978=ORIENTED_EDGE('',*,*,#3560,.T.);
#4979=ORIENTED_EDGE('',*,*,#3562,.T.);
#4980=ORIENTED_EDGE('',*,*,#3563,.T.);
#4981=ORIENTED_EDGE('',*,*,#3564,.T.);
#4982=ORIENTED_EDGE('',*,*,#3565,.F.);
#4983=ORIENTED_EDGE('',*,*,#3566,.T.);
#4984=ORIENTED_EDGE('',*,*,#3567,.T.);
#4985=ORIENTED_EDGE('',*,*,#3568,.T.);
#4986=ORIENTED_EDGE('',*,*,#3563,.F.);
#4987=ORIENTED_EDGE('',*,*,#3569,.T.);
#4988=ORIENTED_EDGE('',*,*,#3570,.T.);
#4989=ORIENTED_EDGE('',*,*,#3571,.T.);
#4990=ORIENTED_EDGE('',*,*,#3567,.F.);
#4991=ORIENTED_EDGE('',*,*,#3572,.T.);
#4992=ORIENTED_EDGE('',*,*,#3573,.T.);
#4993=ORIENTED_EDGE('',*,*,#3574,.T.);
#4994=ORIENTED_EDGE('',*,*,#3570,.F.);
#4995=ORIENTED_EDGE('',*,*,#3575,.T.);
#4996=ORIENTED_EDGE('',*,*,#3576,.T.);
#4997=ORIENTED_EDGE('',*,*,#3577,.T.);
#4998=ORIENTED_EDGE('',*,*,#3573,.F.);
#4999=ORIENTED_EDGE('',*,*,#3578,.T.);
#5000=ORIENTED_EDGE('',*,*,#3565,.T.);
#5001=ORIENTED_EDGE('',*,*,#3579,.T.);
#5002=ORIENTED_EDGE('',*,*,#3576,.F.);
#5003=ORIENTED_EDGE('',*,*,#3578,.F.);
#5004=ORIENTED_EDGE('',*,*,#3575,.F.);
#5005=ORIENTED_EDGE('',*,*,#3572,.F.);
#5006=ORIENTED_EDGE('',*,*,#3569,.F.);
#5007=ORIENTED_EDGE('',*,*,#3566,.F.);
#5008=ORIENTED_EDGE('',*,*,#3562,.F.);
#5009=ORIENTED_EDGE('',*,*,#3579,.F.);
#5010=ORIENTED_EDGE('',*,*,#3564,.F.);
#5011=ORIENTED_EDGE('',*,*,#3568,.F.);
#5012=ORIENTED_EDGE('',*,*,#3571,.F.);
#5013=ORIENTED_EDGE('',*,*,#3574,.F.);
#5014=ORIENTED_EDGE('',*,*,#3577,.F.);
#5015=ORIENTED_EDGE('',*,*,#3580,.F.);
#5016=ORIENTED_EDGE('',*,*,#3581,.F.);
#5017=ORIENTED_EDGE('',*,*,#3582,.F.);
#5018=ORIENTED_EDGE('',*,*,#3583,.F.);
#5019=ORIENTED_EDGE('',*,*,#3584,.F.);
#5020=ORIENTED_EDGE('',*,*,#3585,.F.);
#5021=ORIENTED_EDGE('',*,*,#3586,.F.);
#5022=ORIENTED_EDGE('',*,*,#3587,.F.);
#5023=ORIENTED_EDGE('',*,*,#3584,.T.);
#5024=ORIENTED_EDGE('',*,*,#3588,.T.);
#5025=ORIENTED_EDGE('',*,*,#3589,.T.);
#5026=ORIENTED_EDGE('',*,*,#3590,.T.);
#5027=ORIENTED_EDGE('',*,*,#3583,.T.);
#5028=ORIENTED_EDGE('',*,*,#3591,.F.);
#5029=ORIENTED_EDGE('',*,*,#3592,.T.);
#5030=ORIENTED_EDGE('',*,*,#3588,.F.);
#5031=ORIENTED_EDGE('',*,*,#3582,.T.);
#5032=ORIENTED_EDGE('',*,*,#3593,.T.);
#5033=ORIENTED_EDGE('',*,*,#3594,.T.);
#5034=ORIENTED_EDGE('',*,*,#3591,.T.);
#5035=ORIENTED_EDGE('',*,*,#3581,.T.);
#5036=ORIENTED_EDGE('',*,*,#3595,.F.);
#5037=ORIENTED_EDGE('',*,*,#3596,.T.);
#5038=ORIENTED_EDGE('',*,*,#3593,.F.);
#5039=ORIENTED_EDGE('',*,*,#3597,.F.);
#5040=ORIENTED_EDGE('',*,*,#3598,.F.);
#5041=ORIENTED_EDGE('',*,*,#3589,.F.);
#5042=ORIENTED_EDGE('',*,*,#3592,.F.);
#5043=ORIENTED_EDGE('',*,*,#3594,.F.);
#5044=ORIENTED_EDGE('',*,*,#3596,.F.);
#5045=ORIENTED_EDGE('',*,*,#3599,.F.);
#5046=ORIENTED_EDGE('',*,*,#3600,.F.);
#5047=ORIENTED_EDGE('',*,*,#3585,.T.);
#5048=ORIENTED_EDGE('',*,*,#3590,.F.);
#5049=ORIENTED_EDGE('',*,*,#3598,.T.);
#5050=ORIENTED_EDGE('',*,*,#3601,.F.);
#5051=ORIENTED_EDGE('',*,*,#3580,.T.);
#5052=ORIENTED_EDGE('',*,*,#3602,.T.);
#5053=ORIENTED_EDGE('',*,*,#3599,.T.);
#5054=ORIENTED_EDGE('',*,*,#3595,.T.);
#5055=ORIENTED_EDGE('',*,*,#3586,.T.);
#5056=ORIENTED_EDGE('',*,*,#3601,.T.);
#5057=ORIENTED_EDGE('',*,*,#3597,.T.);
#5058=ORIENTED_EDGE('',*,*,#3603,.T.);
#5059=ORIENTED_EDGE('',*,*,#3587,.T.);
#5060=ORIENTED_EDGE('',*,*,#3603,.F.);
#5061=ORIENTED_EDGE('',*,*,#3600,.T.);
#5062=ORIENTED_EDGE('',*,*,#3602,.F.);
#5063=ORIENTED_EDGE('',*,*,#3604,.F.);
#5064=ORIENTED_EDGE('',*,*,#3605,.T.);
#5065=ORIENTED_EDGE('',*,*,#3606,.T.);
#5066=ORIENTED_EDGE('',*,*,#3607,.F.);
#5067=ORIENTED_EDGE('',*,*,#3608,.F.);
#5068=ORIENTED_EDGE('',*,*,#3609,.T.);
#5069=ORIENTED_EDGE('',*,*,#3610,.T.);
#5070=ORIENTED_EDGE('',*,*,#3605,.F.);
#5071=ORIENTED_EDGE('',*,*,#3611,.F.);
#5072=ORIENTED_EDGE('',*,*,#3612,.T.);
#5073=ORIENTED_EDGE('',*,*,#3613,.T.);
#5074=ORIENTED_EDGE('',*,*,#3609,.F.);
#5075=ORIENTED_EDGE('',*,*,#3614,.F.);
#5076=ORIENTED_EDGE('',*,*,#3615,.T.);
#5077=ORIENTED_EDGE('',*,*,#3616,.T.);
#5078=ORIENTED_EDGE('',*,*,#3612,.F.);
#5079=ORIENTED_EDGE('',*,*,#3617,.F.);
#5080=ORIENTED_EDGE('',*,*,#3618,.T.);
#5081=ORIENTED_EDGE('',*,*,#3619,.T.);
#5082=ORIENTED_EDGE('',*,*,#3615,.F.);
#5083=ORIENTED_EDGE('',*,*,#3620,.F.);
#5084=ORIENTED_EDGE('',*,*,#3607,.T.);
#5085=ORIENTED_EDGE('',*,*,#3621,.T.);
#5086=ORIENTED_EDGE('',*,*,#3618,.F.);
#5087=ORIENTED_EDGE('',*,*,#3621,.F.);
#5088=ORIENTED_EDGE('',*,*,#3606,.F.);
#5089=ORIENTED_EDGE('',*,*,#3610,.F.);
#5090=ORIENTED_EDGE('',*,*,#3613,.F.);
#5091=ORIENTED_EDGE('',*,*,#3616,.F.);
#5092=ORIENTED_EDGE('',*,*,#3619,.F.);
#5093=ORIENTED_EDGE('',*,*,#3622,.F.);
#5094=ORIENTED_EDGE('',*,*,#3604,.T.);
#5095=ORIENTED_EDGE('',*,*,#3620,.T.);
#5096=ORIENTED_EDGE('',*,*,#3617,.T.);
#5097=ORIENTED_EDGE('',*,*,#3614,.T.);
#5098=ORIENTED_EDGE('',*,*,#3611,.T.);
#5099=ORIENTED_EDGE('',*,*,#3608,.T.);
#5100=ORIENTED_EDGE('',*,*,#3623,.F.);
#5101=ORIENTED_EDGE('',*,*,#3624,.T.);
#5102=ORIENTED_EDGE('',*,*,#3622,.T.);
#5103=ORIENTED_EDGE('',*,*,#3624,.F.);
#5104=ORIENTED_EDGE('',*,*,#3625,.F.);
#5105=ORIENTED_EDGE('',*,*,#3626,.T.);
#5106=ORIENTED_EDGE('',*,*,#3623,.T.);
#5107=ORIENTED_EDGE('',*,*,#3626,.F.);
#5108=ORIENTED_EDGE('',*,*,#3627,.F.);
#5109=ORIENTED_EDGE('',*,*,#3628,.T.);
#5110=ORIENTED_EDGE('',*,*,#3625,.T.);
#5111=ORIENTED_EDGE('',*,*,#3628,.F.);
#5112=ORIENTED_EDGE('',*,*,#3627,.T.);
#5113=CYLINDRICAL_SURFACE('',#5880,0.34);
#5114=CYLINDRICAL_SURFACE('',#5883,0.34);
#5115=CYLINDRICAL_SURFACE('',#5886,0.34);
#5116=CYLINDRICAL_SURFACE('',#5889,0.34);
#5117=CYLINDRICAL_SURFACE('',#5913,0.425);
#5118=CYLINDRICAL_SURFACE('',#5916,0.645);
#5119=CYLINDRICAL_SURFACE('',#5922,0.425);
#5120=CYLINDRICAL_SURFACE('',#5925,0.645);
#5121=CYLINDRICAL_SURFACE('',#5931,0.425);
#5122=CYLINDRICAL_SURFACE('',#5934,0.645);
#5123=CYLINDRICAL_SURFACE('',#5940,0.425);
#5124=CYLINDRICAL_SURFACE('',#5943,0.645);
#5125=CYLINDRICAL_SURFACE('',#5950,2.05);
#5126=CYLINDRICAL_SURFACE('',#5953,2.05);
#5127=CYLINDRICAL_SURFACE('',#5971,2.8);
#5128=CYLINDRICAL_SURFACE('',#5981,0.65);
#5129=CYLINDRICAL_SURFACE('',#5983,0.65);
#5130=CYLINDRICAL_SURFACE('',#5991,1.8);
#5131=CYLINDRICAL_SURFACE('',#6000,0.25);
#5132=CYLINDRICAL_SURFACE('',#6001,0.25);
#5133=CYLINDRICAL_SURFACE('',#6002,1.65);
#5134=CYLINDRICAL_SURFACE('',#6005,0.25);
#5135=CYLINDRICAL_SURFACE('',#6006,0.25);
#5136=CYLINDRICAL_SURFACE('',#6007,0.25);
#5137=CYLINDRICAL_SURFACE('',#6008,0.25);
#5138=CYLINDRICAL_SURFACE('',#6013,1.75);
#5139=CYLINDRICAL_SURFACE('',#6017,1.);
#5140=CYLINDRICAL_SURFACE('',#6021,0.42);
#5141=CYLINDRICAL_SURFACE('',#6024,0.8);
#5142=CYLINDRICAL_SURFACE('',#6044,0.65);
#5143=CYLINDRICAL_SURFACE('',#6052,0.3933);
#5144=CYLINDRICAL_SURFACE('',#6079,0.21);
#5145=CYLINDRICAL_SURFACE('',#6083,0.21);
#5146=CYLINDRICAL_SURFACE('',#6101,0.6);
#5147=CYLINDRICAL_SURFACE('',#6105,0.6);
#5148=CYLINDRICAL_SURFACE('',#6109,1.);
#5149=CYLINDRICAL_SURFACE('',#6115,0.605);
#5150=CYLINDRICAL_SURFACE('',#6118,0.9);
#5151=CYLINDRICAL_SURFACE('',#6124,0.605);
#5152=CYLINDRICAL_SURFACE('',#6127,0.9);
#5153=CYLINDRICAL_SURFACE('',#6133,0.605);
#5154=CYLINDRICAL_SURFACE('',#6136,0.9);
#5155=CYLINDRICAL_SURFACE('',#6142,0.275);
#5156=CYLINDRICAL_SURFACE('',#6145,1.);
#5157=CYLINDRICAL_SURFACE('',#6151,0.275);
#5158=CYLINDRICAL_SURFACE('',#6154,1.);
#5159=CYLINDRICAL_SURFACE('',#6162,0.21);
#5160=CYLINDRICAL_SURFACE('',#6172,1.);
#5161=CYLINDRICAL_SURFACE('',#6174,2.);
#5162=CYLINDRICAL_SURFACE('',#6180,0.21);
#5163=CYLINDRICAL_SURFACE('',#6184,1.005);
#5164=CYLINDRICAL_SURFACE('',#6187,1.5);
#5165=CYLINDRICAL_SURFACE('',#6195,0.21);
#5166=CYLINDRICAL_SURFACE('',#6199,1.005);
#5167=CYLINDRICAL_SURFACE('',#6202,1.5);
#5168=CYLINDRICAL_SURFACE('',#6215,0.6);
#5169=CYLINDRICAL_SURFACE('',#6217,0.125);
#5170=CYLINDRICAL_SURFACE('',#6218,0.125);
#5171=CYLINDRICAL_SURFACE('',#6219,1.);
#5172=CYLINDRICAL_SURFACE('',#6222,0.125);
#5173=CYLINDRICAL_SURFACE('',#6223,0.125);
#5174=CYLINDRICAL_SURFACE('',#6307,1.4);
#5175=CYLINDRICAL_SURFACE('',#6392,1.4);
#5176=CYLINDRICAL_SURFACE('',#6393,0.0555000000000001);
#5177=CYLINDRICAL_SURFACE('',#6394,1.24783954473516);
#5178=CYLINDRICAL_SURFACE('',#6395,0.0555000000000001);
#5179=CYLINDRICAL_SURFACE('',#6396,1.24783954473516);
#5180=CYLINDRICAL_SURFACE('',#6397,0.0555000000000001);
#5181=CYLINDRICAL_SURFACE('',#6398,1.24783954473516);
#5182=CYLINDRICAL_SURFACE('',#6399,0.0555000000000001);
#5183=CYLINDRICAL_SURFACE('',#6400,1.24783954473516);
#5184=CYLINDRICAL_SURFACE('',#6401,0.0555000000000001);
#5185=CYLINDRICAL_SURFACE('',#6402,1.24783954473516);
#5186=CYLINDRICAL_SURFACE('',#6403,0.0555000000000001);
#5187=CYLINDRICAL_SURFACE('',#6404,1.24783954473516);
#5188=CYLINDRICAL_SURFACE('',#6405,0.0555000000000001);
#5189=CYLINDRICAL_SURFACE('',#6406,1.24783954473516);
#5190=CYLINDRICAL_SURFACE('',#6407,0.0555000000000001);
#5191=CYLINDRICAL_SURFACE('',#6408,1.24783954473516);
#5192=CYLINDRICAL_SURFACE('',#6409,0.0555000000000001);
#5193=CYLINDRICAL_SURFACE('',#6410,1.24783954473516);
#5194=CYLINDRICAL_SURFACE('',#6411,0.0555000000000001);
#5195=CYLINDRICAL_SURFACE('',#6412,1.24783954473516);
#5196=CYLINDRICAL_SURFACE('',#6413,0.0555000000000001);
#5197=CYLINDRICAL_SURFACE('',#6414,1.24783954473516);
#5198=CYLINDRICAL_SURFACE('',#6415,0.0555000000000001);
#5199=CYLINDRICAL_SURFACE('',#6416,1.24783954473516);
#5200=CYLINDRICAL_SURFACE('',#6417,0.0555000000000001);
#5201=CYLINDRICAL_SURFACE('',#6418,1.24783954473516);
#5202=CYLINDRICAL_SURFACE('',#6419,0.0555000000000001);
#5203=CYLINDRICAL_SURFACE('',#6420,1.24783954473516);
#5204=CYLINDRICAL_SURFACE('',#6421,0.0555000000000001);
#5205=CYLINDRICAL_SURFACE('',#6422,1.24783954473516);
#5206=CYLINDRICAL_SURFACE('',#6423,0.0555000000000001);
#5207=CYLINDRICAL_SURFACE('',#6424,1.24783954473516);
#5208=CYLINDRICAL_SURFACE('',#6425,0.0555000000000001);
#5209=CYLINDRICAL_SURFACE('',#6426,1.24783954473516);
#5210=CYLINDRICAL_SURFACE('',#6427,0.0555000000000001);
#5211=CYLINDRICAL_SURFACE('',#6428,1.24783954473516);
#5212=CYLINDRICAL_SURFACE('',#6429,0.0555000000000001);
#5213=CYLINDRICAL_SURFACE('',#6430,1.24783954473516);
#5214=CYLINDRICAL_SURFACE('',#6431,0.0555000000000001);
#5215=CYLINDRICAL_SURFACE('',#6432,1.24783954473516);
#5216=CYLINDRICAL_SURFACE('',#6433,0.0555000000000001);
#5217=CYLINDRICAL_SURFACE('',#6434,1.24783954473516);
#5218=CYLINDRICAL_SURFACE('',#6435,0.0555000000000001);
#5219=CYLINDRICAL_SURFACE('',#6436,1.24783954473516);
#5220=CYLINDRICAL_SURFACE('',#6437,0.0555000000000001);
#5221=CYLINDRICAL_SURFACE('',#6438,1.24783954473516);
#5222=CYLINDRICAL_SURFACE('',#6439,0.0555000000000001);
#5223=CYLINDRICAL_SURFACE('',#6440,1.24783954473516);
#5224=CYLINDRICAL_SURFACE('',#6441,0.0555000000000001);
#5225=CYLINDRICAL_SURFACE('',#6442,1.24783954473516);
#5226=CYLINDRICAL_SURFACE('',#6443,0.0555000000000001);
#5227=CYLINDRICAL_SURFACE('',#6444,1.24783954473516);
#5228=CYLINDRICAL_SURFACE('',#6445,0.0555000000000001);
#5229=CYLINDRICAL_SURFACE('',#6446,1.24783954473516);
#5230=CYLINDRICAL_SURFACE('',#6447,0.0555000000000001);
#5231=CYLINDRICAL_SURFACE('',#6448,1.24783954473516);
#5232=CYLINDRICAL_SURFACE('',#6449,0.0555000000000001);
#5233=CYLINDRICAL_SURFACE('',#6450,1.24783954473516);
#5234=CYLINDRICAL_SURFACE('',#6451,0.0555000000000001);
#5235=CYLINDRICAL_SURFACE('',#6452,1.24783954473516);
#5236=CYLINDRICAL_SURFACE('',#6453,0.0555000000000001);
#5237=CYLINDRICAL_SURFACE('',#6454,1.24783954473516);
#5238=CYLINDRICAL_SURFACE('',#6455,0.0555000000000001);
#5239=CYLINDRICAL_SURFACE('',#6456,1.24783954473516);
#5240=CYLINDRICAL_SURFACE('',#6457,0.0555000000000001);
#5241=CYLINDRICAL_SURFACE('',#6458,1.24783954473516);
#5242=CYLINDRICAL_SURFACE('',#6459,0.0555000000000001);
#5243=CYLINDRICAL_SURFACE('',#6460,1.24783954473516);
#5244=CYLINDRICAL_SURFACE('',#6461,0.0555000000000001);
#5245=CYLINDRICAL_SURFACE('',#6462,1.24783954473516);
#5246=CYLINDRICAL_SURFACE('',#6463,0.0555000000000001);
#5247=CYLINDRICAL_SURFACE('',#6464,1.24783954473516);
#5248=CYLINDRICAL_SURFACE('',#6465,0.0555000000000001);
#5249=CYLINDRICAL_SURFACE('',#6466,1.24783954473516);
#5250=CYLINDRICAL_SURFACE('',#6467,0.0555000000000001);
#5251=CYLINDRICAL_SURFACE('',#6468,1.24783954473516);
#5252=CYLINDRICAL_SURFACE('',#6469,0.0555000000000001);
#5253=CYLINDRICAL_SURFACE('',#6470,1.24783954473516);
#5254=CYLINDRICAL_SURFACE('',#6471,0.0555000000000001);
#5255=CYLINDRICAL_SURFACE('',#6472,1.24783954473516);
#5256=CYLINDRICAL_SURFACE('',#6489,0.425);
#5257=CYLINDRICAL_SURFACE('',#6497,0.24505);
#5258=CYLINDRICAL_SURFACE('',#6533,0.24505);
#5259=ADVANCED_FACE('',(#588),#5113,.F.);
#5260=ADVANCED_FACE('',(#589),#5114,.F.);
#5261=ADVANCED_FACE('',(#590),#5115,.F.);
#5262=ADVANCED_FACE('',(#591),#5116,.F.);
#5263=ADVANCED_FACE('',(#592),#431,.T.);
#5264=ADVANCED_FACE('',(#593),#432,.T.);
#5265=ADVANCED_FACE('',(#594),#433,.T.);
#5266=ADVANCED_FACE('',(#595),#434,.T.);
#5267=ADVANCED_FACE('',(#596,#340,#341,#342,#343),#435,.T.);
#5268=ADVANCED_FACE('',(#597,#344,#345,#346,#347),#436,.F.);
#5269=ADVANCED_FACE('',(#598),#437,.T.);
#5270=ADVANCED_FACE('',(#599),#438,.T.);
#5271=ADVANCED_FACE('',(#600),#439,.T.);
#5272=ADVANCED_FACE('',(#601),#440,.T.);
#5273=ADVANCED_FACE('',(#602),#441,.T.);
#5274=ADVANCED_FACE('',(#603),#442,.F.);
#5275=ADVANCED_FACE('',(#604),#443,.T.);
#5276=ADVANCED_FACE('',(#605),#444,.T.);
#5277=ADVANCED_FACE('',(#606),#445,.T.);
#5278=ADVANCED_FACE('',(#607),#446,.T.);
#5279=ADVANCED_FACE('',(#608),#447,.T.);
#5280=ADVANCED_FACE('',(#609),#448,.F.);
#5281=ADVANCED_FACE('',(#610),#5117,.F.);
#5282=ADVANCED_FACE('',(#611),#5118,.T.);
#5283=ADVANCED_FACE('',(#612,#348),#449,.T.);
#5284=ADVANCED_FACE('',(#613,#349),#450,.F.);
#5285=ADVANCED_FACE('',(#614),#5119,.F.);
#5286=ADVANCED_FACE('',(#615),#5120,.T.);
#5287=ADVANCED_FACE('',(#616,#350),#451,.T.);
#5288=ADVANCED_FACE('',(#617,#351),#452,.F.);
#5289=ADVANCED_FACE('',(#618),#5121,.F.);
#5290=ADVANCED_FACE('',(#619),#5122,.T.);
#5291=ADVANCED_FACE('',(#620,#352),#453,.T.);
#5292=ADVANCED_FACE('',(#621,#353),#454,.F.);
#5293=ADVANCED_FACE('',(#622),#5123,.F.);
#5294=ADVANCED_FACE('',(#623),#5124,.T.);
#5295=ADVANCED_FACE('',(#624,#354),#455,.T.);
#5296=ADVANCED_FACE('',(#625,#355),#456,.F.);
#5297=ADVANCED_FACE('',(#626),#5125,.F.);
#5298=ADVANCED_FACE('',(#627),#5126,.F.);
#5299=ADVANCED_FACE('',(#628,#356,#357),#238,.F.);
#5300=ADVANCED_FACE('',(#629),#457,.T.);
#5301=ADVANCED_FACE('',(#630),#458,.T.);
#5302=ADVANCED_FACE('',(#631),#459,.T.);
#5303=ADVANCED_FACE('',(#632),#460,.T.);
#5304=ADVANCED_FACE('',(#633),#461,.T.);
#5305=ADVANCED_FACE('',(#634),#462,.T.);
#5306=ADVANCED_FACE('',(#635,#358,#359,#360),#463,.T.);
#5307=ADVANCED_FACE('',(#636),#5127,.T.);
#5308=ADVANCED_FACE('',(#637,#361),#464,.F.);
#5309=ADVANCED_FACE('',(#638,#362),#465,.T.);
#5310=ADVANCED_FACE('',(#639),#466,.F.);
#5311=ADVANCED_FACE('',(#640),#467,.F.);
#5312=ADVANCED_FACE('',(#641),#468,.F.);
#5313=ADVANCED_FACE('',(#642),#469,.F.);
#5314=ADVANCED_FACE('',(#643),#470,.F.);
#5315=ADVANCED_FACE('',(#644),#5128,.F.);
#5316=ADVANCED_FACE('',(#645),#5129,.F.);
#5317=ADVANCED_FACE('',(#646),#471,.T.);
#5318=ADVANCED_FACE('',(#647),#472,.T.);
#5319=ADVANCED_FACE('',(#648),#473,.T.);
#5320=ADVANCED_FACE('',(#649),#474,.T.);
#5321=ADVANCED_FACE('',(#650,#363,#364,#365),#475,.F.);
#5322=ADVANCED_FACE('',(#651),#5130,.F.);
#5323=ADVANCED_FACE('',(#652,#366),#476,.T.);
#5324=ADVANCED_FACE('',(#653,#367,#368),#239,.T.);
#5325=ADVANCED_FACE('',(#654,#369),#477,.T.);
#5326=ADVANCED_FACE('',(#655),#5131,.F.);
#5327=ADVANCED_FACE('',(#656),#5132,.F.);
#5328=ADVANCED_FACE('',(#657,#370,#371,#372,#373,#374,#375),#5133,.T.);
#5329=ADVANCED_FACE('',(#658),#5134,.F.);
#5330=ADVANCED_FACE('',(#659),#5135,.F.);
#5331=ADVANCED_FACE('',(#660),#5136,.F.);
#5332=ADVANCED_FACE('',(#661),#5137,.F.);
#5333=ADVANCED_FACE('',(#662,#376),#478,.T.);
#5334=ADVANCED_FACE('',(#663,#377),#479,.T.);
#5335=ADVANCED_FACE('',(#664),#5138,.T.);
#5336=ADVANCED_FACE('',(#665,#378),#480,.T.);
#5337=ADVANCED_FACE('',(#666,#379,#380,#381,#382,#383,#384),#5139,.F.);
#5338=ADVANCED_FACE('',(#667),#5140,.F.);
#5339=ADVANCED_FACE('',(#668),#5141,.T.);
#5340=ADVANCED_FACE('',(#669,#385),#481,.T.);
#5341=ADVANCED_FACE('',(#670,#386),#482,.F.);
#5342=ADVANCED_FACE('',(#671),#483,.F.);
#5343=ADVANCED_FACE('',(#672),#484,.F.);
#5344=ADVANCED_FACE('',(#673),#485,.F.);
#5345=ADVANCED_FACE('',(#674),#486,.F.);
#5346=ADVANCED_FACE('',(#675),#487,.F.);
#5347=ADVANCED_FACE('',(#676),#488,.F.);
#5348=ADVANCED_FACE('',(#677),#489,.F.);
#5349=ADVANCED_FACE('',(#678),#490,.F.);
#5350=ADVANCED_FACE('',(#679),#491,.F.);
#5351=ADVANCED_FACE('',(#680),#492,.T.);
#5352=ADVANCED_FACE('',(#681),#11,.T.);
#5353=ADVANCED_FACE('',(#682),#5142,.T.);
#5354=ADVANCED_FACE('',(#683),#12,.T.);
#5355=ADVANCED_FACE('',(#684,#387),#493,.T.);
#5356=ADVANCED_FACE('',(#685),#13,.T.);
#5357=ADVANCED_FACE('',(#686),#5143,.T.);
#5358=ADVANCED_FACE('',(#687),#494,.F.);
#5359=ADVANCED_FACE('',(#688),#495,.T.);
#5360=ADVANCED_FACE('',(#689),#496,.F.);
#5361=ADVANCED_FACE('',(#690),#497,.F.);
#5362=ADVANCED_FACE('',(#691),#498,.F.);
#5363=ADVANCED_FACE('',(#692),#5144,.F.);
#5364=ADVANCED_FACE('',(#693),#499,.T.);
#5365=ADVANCED_FACE('',(#694),#5145,.F.);
#5366=ADVANCED_FACE('',(#695),#500,.F.);
#5367=ADVANCED_FACE('',(#696),#501,.F.);
#5368=ADVANCED_FACE('',(#697),#502,.T.);
#5369=ADVANCED_FACE('',(#698),#503,.F.);
#5370=ADVANCED_FACE('',(#699),#504,.F.);
#5371=ADVANCED_FACE('',(#700),#505,.F.);
#5372=ADVANCED_FACE('',(#701),#506,.F.);
#5373=ADVANCED_FACE('',(#702),#507,.T.);
#5374=ADVANCED_FACE('',(#703),#508,.F.);
#5375=ADVANCED_FACE('',(#704),#509,.F.);
#5376=ADVANCED_FACE('',(#705),#510,.F.);
#5377=ADVANCED_FACE('',(#706,#388),#5146,.T.);
#5378=ADVANCED_FACE('',(#707,#389),#511,.T.);
#5379=ADVANCED_FACE('',(#708,#390),#5147,.T.);
#5380=ADVANCED_FACE('',(#709,#391),#512,.F.);
#5381=ADVANCED_FACE('',(#710,#392),#5148,.T.);
#5382=ADVANCED_FACE('',(#711,#393),#513,.T.);
#5383=ADVANCED_FACE('',(#712,#394),#514,.F.);
#5384=ADVANCED_FACE('',(#713),#5149,.F.);
#5385=ADVANCED_FACE('',(#714),#5150,.T.);
#5386=ADVANCED_FACE('',(#715,#395),#515,.T.);
#5387=ADVANCED_FACE('',(#716,#396),#516,.F.);
#5388=ADVANCED_FACE('',(#717),#5151,.F.);
#5389=ADVANCED_FACE('',(#718),#5152,.T.);
#5390=ADVANCED_FACE('',(#719,#397),#517,.T.);
#5391=ADVANCED_FACE('',(#720,#398),#518,.F.);
#5392=ADVANCED_FACE('',(#721),#5153,.F.);
#5393=ADVANCED_FACE('',(#722),#5154,.T.);
#5394=ADVANCED_FACE('',(#723,#399),#519,.T.);
#5395=ADVANCED_FACE('',(#724,#400),#520,.F.);
#5396=ADVANCED_FACE('',(#725),#5155,.F.);
#5397=ADVANCED_FACE('',(#726),#5156,.T.);
#5398=ADVANCED_FACE('',(#727,#401),#521,.T.);
#5399=ADVANCED_FACE('',(#728,#402),#522,.F.);
#5400=ADVANCED_FACE('',(#729),#5157,.F.);
#5401=ADVANCED_FACE('',(#730),#5158,.T.);
#5402=ADVANCED_FACE('',(#731,#403),#523,.T.);
#5403=ADVANCED_FACE('',(#732,#404),#524,.F.);
#5404=ADVANCED_FACE('',(#733),#525,.T.);
#5405=ADVANCED_FACE('',(#734),#5159,.F.);
#5406=ADVANCED_FACE('',(#735),#526,.T.);
#5407=ADVANCED_FACE('',(#736),#527,.F.);
#5408=ADVANCED_FACE('',(#737),#528,.F.);
#5409=ADVANCED_FACE('',(#738),#529,.F.);
#5410=ADVANCED_FACE('',(#739,#405),#530,.T.);
#5411=ADVANCED_FACE('',(#740,#406),#5160,.F.);
#5412=ADVANCED_FACE('',(#741,#407),#5161,.T.);
#5413=ADVANCED_FACE('',(#742,#408),#531,.F.);
#5414=ADVANCED_FACE('',(#743),#532,.T.);
#5415=ADVANCED_FACE('',(#744),#5162,.F.);
#5416=ADVANCED_FACE('',(#745),#533,.T.);
#5417=ADVANCED_FACE('',(#746,#409),#5163,.F.);
#5418=ADVANCED_FACE('',(#747,#410),#5164,.T.);
#5419=ADVANCED_FACE('',(#748,#411),#534,.T.);
#5420=ADVANCED_FACE('',(#749,#412),#535,.F.);
#5421=ADVANCED_FACE('',(#750),#536,.T.);
#5422=ADVANCED_FACE('',(#751),#5165,.F.);
#5423=ADVANCED_FACE('',(#752),#537,.T.);
#5424=ADVANCED_FACE('',(#753,#413),#5166,.F.);
#5425=ADVANCED_FACE('',(#754,#414),#5167,.T.);
#5426=ADVANCED_FACE('',(#755,#415),#538,.T.);
#5427=ADVANCED_FACE('',(#756,#416),#539,.F.);
#5428=ADVANCED_FACE('',(#757),#540,.F.);
#5429=ADVANCED_FACE('',(#758,#417),#541,.F.);
#5430=ADVANCED_FACE('',(#759),#542,.F.);
#5431=ADVANCED_FACE('',(#760,#418),#543,.T.);
#5432=ADVANCED_FACE('',(#761,#419,#420,#421),#5168,.F.);
#5433=ADVANCED_FACE('',(#762),#5169,.F.);
#5434=ADVANCED_FACE('',(#763),#5170,.F.);
#5435=ADVANCED_FACE('',(#764,#422,#423,#424),#5171,.T.);
#5436=ADVANCED_FACE('',(#765),#5172,.F.);
#5437=ADVANCED_FACE('',(#766),#5173,.F.);
#5438=ADVANCED_FACE('',(#767,#425),#544,.F.);
#5439=ADVANCED_FACE('',(#768,#426),#545,.T.);
#5440=ADVANCED_FACE('',(#769),#5174,.T.);
#5441=ADVANCED_FACE('',(#770,#427),#546,.F.);
#5442=ADVANCED_FACE('',(#771,#428),#547,.F.);
#5443=ADVANCED_FACE('',(#772),#5175,.T.);
#5444=ADVANCED_FACE('',(#773),#5176,.F.);
#5445=ADVANCED_FACE('',(#774),#5177,.T.);
#5446=ADVANCED_FACE('',(#775),#5178,.F.);
#5447=ADVANCED_FACE('',(#776),#5179,.T.);
#5448=ADVANCED_FACE('',(#777),#5180,.F.);
#5449=ADVANCED_FACE('',(#778),#5181,.T.);
#5450=ADVANCED_FACE('',(#779),#5182,.F.);
#5451=ADVANCED_FACE('',(#780),#5183,.T.);
#5452=ADVANCED_FACE('',(#781),#5184,.F.);
#5453=ADVANCED_FACE('',(#782),#5185,.T.);
#5454=ADVANCED_FACE('',(#783),#5186,.F.);
#5455=ADVANCED_FACE('',(#784),#5187,.T.);
#5456=ADVANCED_FACE('',(#785),#5188,.F.);
#5457=ADVANCED_FACE('',(#786),#5189,.T.);
#5458=ADVANCED_FACE('',(#787),#5190,.F.);
#5459=ADVANCED_FACE('',(#788),#5191,.T.);
#5460=ADVANCED_FACE('',(#789),#5192,.F.);
#5461=ADVANCED_FACE('',(#790),#5193,.T.);
#5462=ADVANCED_FACE('',(#791),#5194,.F.);
#5463=ADVANCED_FACE('',(#792),#5195,.T.);
#5464=ADVANCED_FACE('',(#793),#5196,.F.);
#5465=ADVANCED_FACE('',(#794),#5197,.T.);
#5466=ADVANCED_FACE('',(#795),#5198,.F.);
#5467=ADVANCED_FACE('',(#796),#5199,.T.);
#5468=ADVANCED_FACE('',(#797),#5200,.F.);
#5469=ADVANCED_FACE('',(#798),#5201,.T.);
#5470=ADVANCED_FACE('',(#799),#5202,.F.);
#5471=ADVANCED_FACE('',(#800),#5203,.T.);
#5472=ADVANCED_FACE('',(#801),#5204,.F.);
#5473=ADVANCED_FACE('',(#802),#5205,.T.);
#5474=ADVANCED_FACE('',(#803),#5206,.F.);
#5475=ADVANCED_FACE('',(#804),#5207,.T.);
#5476=ADVANCED_FACE('',(#805),#5208,.F.);
#5477=ADVANCED_FACE('',(#806),#5209,.T.);
#5478=ADVANCED_FACE('',(#807),#5210,.F.);
#5479=ADVANCED_FACE('',(#808),#5211,.T.);
#5480=ADVANCED_FACE('',(#809),#5212,.F.);
#5481=ADVANCED_FACE('',(#810),#5213,.T.);
#5482=ADVANCED_FACE('',(#811),#5214,.F.);
#5483=ADVANCED_FACE('',(#812),#5215,.T.);
#5484=ADVANCED_FACE('',(#813),#5216,.F.);
#5485=ADVANCED_FACE('',(#814),#5217,.T.);
#5486=ADVANCED_FACE('',(#815),#5218,.F.);
#5487=ADVANCED_FACE('',(#816),#5219,.T.);
#5488=ADVANCED_FACE('',(#817),#5220,.F.);
#5489=ADVANCED_FACE('',(#818),#5221,.T.);
#5490=ADVANCED_FACE('',(#819),#5222,.F.);
#5491=ADVANCED_FACE('',(#820),#5223,.T.);
#5492=ADVANCED_FACE('',(#821),#5224,.F.);
#5493=ADVANCED_FACE('',(#822),#5225,.T.);
#5494=ADVANCED_FACE('',(#823),#5226,.F.);
#5495=ADVANCED_FACE('',(#824),#5227,.T.);
#5496=ADVANCED_FACE('',(#825),#5228,.F.);
#5497=ADVANCED_FACE('',(#826),#5229,.T.);
#5498=ADVANCED_FACE('',(#827),#5230,.F.);
#5499=ADVANCED_FACE('',(#828),#5231,.T.);
#5500=ADVANCED_FACE('',(#829),#5232,.F.);
#5501=ADVANCED_FACE('',(#830),#5233,.T.);
#5502=ADVANCED_FACE('',(#831),#5234,.F.);
#5503=ADVANCED_FACE('',(#832),#5235,.T.);
#5504=ADVANCED_FACE('',(#833),#5236,.F.);
#5505=ADVANCED_FACE('',(#834),#5237,.T.);
#5506=ADVANCED_FACE('',(#835),#5238,.F.);
#5507=ADVANCED_FACE('',(#836),#5239,.T.);
#5508=ADVANCED_FACE('',(#837),#5240,.F.);
#5509=ADVANCED_FACE('',(#838),#5241,.T.);
#5510=ADVANCED_FACE('',(#839),#5242,.F.);
#5511=ADVANCED_FACE('',(#840),#5243,.T.);
#5512=ADVANCED_FACE('',(#841),#5244,.F.);
#5513=ADVANCED_FACE('',(#842),#5245,.T.);
#5514=ADVANCED_FACE('',(#843),#5246,.F.);
#5515=ADVANCED_FACE('',(#844),#5247,.T.);
#5516=ADVANCED_FACE('',(#845),#5248,.F.);
#5517=ADVANCED_FACE('',(#846),#5249,.T.);
#5518=ADVANCED_FACE('',(#847),#5250,.F.);
#5519=ADVANCED_FACE('',(#848),#5251,.T.);
#5520=ADVANCED_FACE('',(#849),#5252,.F.);
#5521=ADVANCED_FACE('',(#850),#5253,.T.);
#5522=ADVANCED_FACE('',(#851),#5254,.F.);
#5523=ADVANCED_FACE('',(#852),#5255,.T.);
#5524=ADVANCED_FACE('',(#853),#548,.T.);
#5525=ADVANCED_FACE('',(#854),#549,.T.);
#5526=ADVANCED_FACE('',(#855),#550,.T.);
#5527=ADVANCED_FACE('',(#856),#551,.T.);
#5528=ADVANCED_FACE('',(#857),#552,.T.);
#5529=ADVANCED_FACE('',(#858),#553,.F.);
#5530=ADVANCED_FACE('',(#859),#554,.T.);
#5531=ADVANCED_FACE('',(#860),#555,.T.);
#5532=ADVANCED_FACE('',(#861),#556,.T.);
#5533=ADVANCED_FACE('',(#862),#557,.F.);
#5534=ADVANCED_FACE('',(#863),#558,.T.);
#5535=ADVANCED_FACE('',(#864),#14,.T.);
#5536=ADVANCED_FACE('',(#865),#5256,.T.);
#5537=ADVANCED_FACE('',(#866),#15,.T.);
#5538=ADVANCED_FACE('',(#867,#429),#559,.T.);
#5539=ADVANCED_FACE('',(#868),#16,.T.);
#5540=ADVANCED_FACE('',(#869),#5257,.T.);
#5541=ADVANCED_FACE('',(#870),#17,.T.);
#5542=ADVANCED_FACE('',(#871),#560,.T.);
#5543=ADVANCED_FACE('',(#872),#561,.F.);
#5544=ADVANCED_FACE('',(#873),#562,.F.);
#5545=ADVANCED_FACE('',(#874),#563,.F.);
#5546=ADVANCED_FACE('',(#875),#564,.F.);
#5547=ADVANCED_FACE('',(#876),#565,.F.);
#5548=ADVANCED_FACE('',(#877),#566,.F.);
#5549=ADVANCED_FACE('',(#878),#567,.F.);
#5550=ADVANCED_FACE('',(#879),#568,.F.);
#5551=ADVANCED_FACE('',(#880),#569,.F.);
#5552=ADVANCED_FACE('',(#881),#570,.T.);
#5553=ADVANCED_FACE('',(#882),#571,.T.);
#5554=ADVANCED_FACE('',(#883),#572,.T.);
#5555=ADVANCED_FACE('',(#884),#573,.T.);
#5556=ADVANCED_FACE('',(#885),#574,.T.);
#5557=ADVANCED_FACE('',(#886),#575,.F.);
#5558=ADVANCED_FACE('',(#887),#576,.T.);
#5559=ADVANCED_FACE('',(#888),#577,.T.);
#5560=ADVANCED_FACE('',(#889),#578,.T.);
#5561=ADVANCED_FACE('',(#890),#579,.F.);
#5562=ADVANCED_FACE('',(#891),#580,.F.);
#5563=ADVANCED_FACE('',(#892),#581,.F.);
#5564=ADVANCED_FACE('',(#893),#582,.F.);
#5565=ADVANCED_FACE('',(#894),#583,.F.);
#5566=ADVANCED_FACE('',(#895),#584,.F.);
#5567=ADVANCED_FACE('',(#896),#585,.F.);
#5568=ADVANCED_FACE('',(#897,#430),#586,.T.);
#5569=ADVANCED_FACE('',(#898),#18,.T.);
#5570=ADVANCED_FACE('',(#899),#5258,.T.);
#5571=ADVANCED_FACE('',(#900),#19,.T.);
#5572=ADVANCED_FACE('',(#901),#587,.T.);
#5573=CLOSED_SHELL('',(#5259,#5260,#5261,#5262,#5263,#5264,#5265,#5266,
#5267,#5268));
#5574=CLOSED_SHELL('',(#5269,#5270,#5271,#5272,#5273,#5274));
#5575=CLOSED_SHELL('',(#5275,#5276,#5277,#5278,#5279,#5280));
#5576=CLOSED_SHELL('',(#5281,#5282,#5283,#5284));
#5577=CLOSED_SHELL('',(#5285,#5286,#5287,#5288));
#5578=CLOSED_SHELL('',(#5289,#5290,#5291,#5292));
#5579=CLOSED_SHELL('',(#5293,#5294,#5295,#5296));
#5580=CLOSED_SHELL('',(#5297,#5298,#5299,#5300,#5301,#5302,#5303,#5304,
#5305,#5306,#5307,#5308,#5309,#5310,#5311,#5312,#5313,#5314,#5315,#5316,
#5317,#5318,#5319,#5320,#5321));
#5581=CLOSED_SHELL('',(#5322,#5323,#5324,#5325));
#5582=CLOSED_SHELL('',(#5326,#5327,#5328,#5329,#5330,#5331,#5332,#5333,
#5334,#5335,#5336,#5337));
#5583=CLOSED_SHELL('',(#5338,#5339,#5340,#5341));
#5584=CLOSED_SHELL('',(#5342,#5343,#5344,#5345,#5346,#5347,#5348,#5349));
#5585=CLOSED_SHELL('',(#5350,#5351,#5352,#5353,#5354,#5355,#5356,#5357));
#5586=CLOSED_SHELL('',(#5358,#5359,#5360,#5361,#5362,#5363,#5364,#5365,
#5366,#5367,#5368,#5369,#5370,#5371,#5372,#5373,#5374,#5375,#5376,#5377,
#5378,#5379,#5380,#5381,#5382,#5383));
#5587=CLOSED_SHELL('',(#5384,#5385,#5386,#5387));
#5588=CLOSED_SHELL('',(#5388,#5389,#5390,#5391));
#5589=CLOSED_SHELL('',(#5392,#5393,#5394,#5395));
#5590=CLOSED_SHELL('',(#5396,#5397,#5398,#5399));
#5591=CLOSED_SHELL('',(#5400,#5401,#5402,#5403));
#5592=CLOSED_SHELL('',(#5404,#5405,#5406,#5407,#5408,#5409,#5410,#5411,
#5412,#5413));
#5593=CLOSED_SHELL('',(#5414,#5415,#5416,#5417,#5418,#5419,#5420));
#5594=CLOSED_SHELL('',(#5421,#5422,#5423,#5424,#5425,#5426,#5427));
#5595=CLOSED_SHELL('',(#5428,#5429,#5430,#5431,#5432,#5433,#5434,#5435,
#5436,#5437,#5438,#5439,#5440,#5441,#5442,#5443,#5444,#5445,#5446,#5447,
#5448,#5449,#5450,#5451,#5452,#5453,#5454,#5455,#5456,#5457,#5458,#5459,
#5460,#5461,#5462,#5463,#5464,#5465,#5466,#5467,#5468,#5469,#5470,#5471,
#5472,#5473,#5474,#5475,#5476,#5477,#5478,#5479,#5480,#5481,#5482,#5483,
#5484,#5485,#5486,#5487,#5488,#5489,#5490,#5491,#5492,#5493,#5494,#5495,
#5496,#5497,#5498,#5499,#5500,#5501,#5502,#5503,#5504,#5505,#5506,#5507,
#5508,#5509,#5510,#5511,#5512,#5513,#5514,#5515,#5516,#5517,#5518,#5519,
#5520,#5521,#5522,#5523));
#5596=CLOSED_SHELL('',(#5524,#5525,#5526,#5527,#5528,#5529,#5530,#5531,
#5532,#5533));
#5597=CLOSED_SHELL('',(#5534,#5535,#5536,#5537,#5538,#5539,#5540,#5541,
#5542));
#5598=CLOSED_SHELL('',(#5543,#5544,#5545,#5546,#5547,#5548,#5549,#5550));
#5599=CLOSED_SHELL('',(#5551,#5552,#5553,#5554,#5555,#5556,#5557,#5558,
#5559,#5560));
#5600=CLOSED_SHELL('',(#5561,#5562,#5563,#5564,#5565,#5566,#5567,#5568,
#5569,#5570,#5571,#5572));
#5601=DERIVED_UNIT_ELEMENT(#5651,1.);
#5602=DERIVED_UNIT_ELEMENT(#10823,-3.);
#5603=DERIVED_UNIT_ELEMENT(#5651,1.);
#5604=DERIVED_UNIT_ELEMENT(#10823,-3.);
#5605=DERIVED_UNIT_ELEMENT(#5651,1.);
#5606=DERIVED_UNIT_ELEMENT(#10823,-3.);
#5607=DERIVED_UNIT_ELEMENT(#5651,1.);
#5608=DERIVED_UNIT_ELEMENT(#10823,-3.);
#5609=DERIVED_UNIT_ELEMENT(#5651,1.);
#5610=DERIVED_UNIT_ELEMENT(#10823,-3.);
#5611=DERIVED_UNIT_ELEMENT(#5651,1.);
#5612=DERIVED_UNIT_ELEMENT(#10823,-3.);
#5613=DERIVED_UNIT_ELEMENT(#5651,1.);
#5614=DERIVED_UNIT_ELEMENT(#10823,-3.);
#5615=DERIVED_UNIT_ELEMENT(#5651,1.);
#5616=DERIVED_UNIT_ELEMENT(#10823,-3.);
#5617=DERIVED_UNIT_ELEMENT(#5651,1.);
#5618=DERIVED_UNIT_ELEMENT(#10823,-3.);
#5619=DERIVED_UNIT_ELEMENT(#5651,1.);
#5620=DERIVED_UNIT_ELEMENT(#10823,-3.);
#5621=DERIVED_UNIT_ELEMENT(#5651,1.);
#5622=DERIVED_UNIT_ELEMENT(#10823,-3.);
#5623=DERIVED_UNIT_ELEMENT(#5651,1.);
#5624=DERIVED_UNIT_ELEMENT(#10823,-3.);
#5625=DERIVED_UNIT_ELEMENT(#5651,1.);
#5626=DERIVED_UNIT_ELEMENT(#10823,-3.);
#5627=DERIVED_UNIT_ELEMENT(#5651,1.);
#5628=DERIVED_UNIT_ELEMENT(#10823,-3.);
#5629=DERIVED_UNIT_ELEMENT(#5651,1.);
#5630=DERIVED_UNIT_ELEMENT(#10823,-3.);
#5631=DERIVED_UNIT_ELEMENT(#5651,1.);
#5632=DERIVED_UNIT_ELEMENT(#10823,-3.);
#5633=DERIVED_UNIT_ELEMENT(#5651,1.);
#5634=DERIVED_UNIT_ELEMENT(#10823,-3.);
#5635=DERIVED_UNIT_ELEMENT(#5651,1.);
#5636=DERIVED_UNIT_ELEMENT(#10823,-3.);
#5637=DERIVED_UNIT_ELEMENT(#5651,1.);
#5638=DERIVED_UNIT_ELEMENT(#10823,-3.);
#5639=DERIVED_UNIT_ELEMENT(#5651,1.);
#5640=DERIVED_UNIT_ELEMENT(#10823,-3.);
#5641=DERIVED_UNIT_ELEMENT(#5651,1.);
#5642=DERIVED_UNIT_ELEMENT(#10823,-3.);
#5643=DERIVED_UNIT_ELEMENT(#5651,1.);
#5644=DERIVED_UNIT_ELEMENT(#10823,-3.);
#5645=DERIVED_UNIT_ELEMENT(#5651,1.);
#5646=DERIVED_UNIT_ELEMENT(#10823,-3.);
#5647=DERIVED_UNIT_ELEMENT(#5651,1.);
#5648=DERIVED_UNIT_ELEMENT(#10823,-3.);
#5649=DERIVED_UNIT_ELEMENT(#5651,1.);
#5650=DERIVED_UNIT_ELEMENT(#10823,-3.);
#5651=(
MASS_UNIT()
NAMED_UNIT(*)
SI_UNIT(.KILO.,.GRAM.)
);
#5652=DERIVED_UNIT((#5601,#5602));
#5653=DERIVED_UNIT((#5603,#5604));
#5654=DERIVED_UNIT((#5605,#5606));
#5655=DERIVED_UNIT((#5607,#5608));
#5656=DERIVED_UNIT((#5609,#5610));
#5657=DERIVED_UNIT((#5611,#5612));
#5658=DERIVED_UNIT((#5613,#5614));
#5659=DERIVED_UNIT((#5615,#5616));
#5660=DERIVED_UNIT((#5617,#5618));
#5661=DERIVED_UNIT((#5619,#5620));
#5662=DERIVED_UNIT((#5621,#5622));
#5663=DERIVED_UNIT((#5623,#5624));
#5664=DERIVED_UNIT((#5625,#5626));
#5665=DERIVED_UNIT((#5627,#5628));
#5666=DERIVED_UNIT((#5629,#5630));
#5667=DERIVED_UNIT((#5631,#5632));
#5668=DERIVED_UNIT((#5633,#5634));
#5669=DERIVED_UNIT((#5635,#5636));
#5670=DERIVED_UNIT((#5637,#5638));
#5671=DERIVED_UNIT((#5639,#5640));
#5672=DERIVED_UNIT((#5641,#5642));
#5673=DERIVED_UNIT((#5643,#5644));
#5674=DERIVED_UNIT((#5645,#5646));
#5675=DERIVED_UNIT((#5647,#5648));
#5676=DERIVED_UNIT((#5649,#5650));
#5677=MEASURE_REPRESENTATION_ITEM('density measure',
POSITIVE_RATIO_MEASURE(7850.),#5652);
#5678=MEASURE_REPRESENTATION_ITEM('density measure',
POSITIVE_RATIO_MEASURE(7850.),#5653);
#5679=MEASURE_REPRESENTATION_ITEM('density measure',
POSITIVE_RATIO_MEASURE(7850.),#5654);
#5680=MEASURE_REPRESENTATION_ITEM('density measure',
POSITIVE_RATIO_MEASURE(7850.),#5655);
#5681=MEASURE_REPRESENTATION_ITEM('density measure',
POSITIVE_RATIO_MEASURE(7850.),#5656);
#5682=MEASURE_REPRESENTATION_ITEM('density measure',
POSITIVE_RATIO_MEASURE(7850.),#5657);
#5683=MEASURE_REPRESENTATION_ITEM('density measure',
POSITIVE_RATIO_MEASURE(7850.),#5658);
#5684=MEASURE_REPRESENTATION_ITEM('density measure',
POSITIVE_RATIO_MEASURE(7850.),#5659);
#5685=MEASURE_REPRESENTATION_ITEM('density measure',
POSITIVE_RATIO_MEASURE(7850.),#5660);
#5686=MEASURE_REPRESENTATION_ITEM('density measure',
POSITIVE_RATIO_MEASURE(7850.),#5661);
#5687=MEASURE_REPRESENTATION_ITEM('density measure',
POSITIVE_RATIO_MEASURE(7850.),#5662);
#5688=MEASURE_REPRESENTATION_ITEM('density measure',
POSITIVE_RATIO_MEASURE(7850.),#5663);
#5689=MEASURE_REPRESENTATION_ITEM('density measure',
POSITIVE_RATIO_MEASURE(7850.),#5664);
#5690=MEASURE_REPRESENTATION_ITEM('density measure',
POSITIVE_RATIO_MEASURE(7850.),#5665);
#5691=MEASURE_REPRESENTATION_ITEM('density measure',
POSITIVE_RATIO_MEASURE(7850.),#5666);
#5692=MEASURE_REPRESENTATION_ITEM('density measure',
POSITIVE_RATIO_MEASURE(7850.),#5667);
#5693=MEASURE_REPRESENTATION_ITEM('density measure',
POSITIVE_RATIO_MEASURE(7850.),#5668);
#5694=MEASURE_REPRESENTATION_ITEM('density measure',
POSITIVE_RATIO_MEASURE(7850.),#5669);
#5695=MEASURE_REPRESENTATION_ITEM('density measure',
POSITIVE_RATIO_MEASURE(7850.),#5670);
#5696=MEASURE_REPRESENTATION_ITEM('density measure',
POSITIVE_RATIO_MEASURE(7850.),#5671);
#5697=MEASURE_REPRESENTATION_ITEM('density measure',
POSITIVE_RATIO_MEASURE(7850.),#5672);
#5698=MEASURE_REPRESENTATION_ITEM('density measure',
POSITIVE_RATIO_MEASURE(7850.),#5673);
#5699=MEASURE_REPRESENTATION_ITEM('density measure',
POSITIVE_RATIO_MEASURE(7850.),#5674);
#5700=MEASURE_REPRESENTATION_ITEM('density measure',
POSITIVE_RATIO_MEASURE(7850.),#5675);
#5701=MEASURE_REPRESENTATION_ITEM('density measure',
POSITIVE_RATIO_MEASURE(7850.),#5676);
#5702=PROPERTY_DEFINITION_REPRESENTATION(#5827,#5752);
#5703=PROPERTY_DEFINITION_REPRESENTATION(#5828,#5753);
#5704=PROPERTY_DEFINITION_REPRESENTATION(#5829,#5754);
#5705=PROPERTY_DEFINITION_REPRESENTATION(#5830,#5755);
#5706=PROPERTY_DEFINITION_REPRESENTATION(#5831,#5756);
#5707=PROPERTY_DEFINITION_REPRESENTATION(#5832,#5757);
#5708=PROPERTY_DEFINITION_REPRESENTATION(#5833,#5758);
#5709=PROPERTY_DEFINITION_REPRESENTATION(#5834,#5759);
#5710=PROPERTY_DEFINITION_REPRESENTATION(#5835,#5760);
#5711=PROPERTY_DEFINITION_REPRESENTATION(#5836,#5761);
#5712=PROPERTY_DEFINITION_REPRESENTATION(#5837,#5762);
#5713=PROPERTY_DEFINITION_REPRESENTATION(#5838,#5763);
#5714=PROPERTY_DEFINITION_REPRESENTATION(#5839,#5764);
#5715=PROPERTY_DEFINITION_REPRESENTATION(#5840,#5765);
#5716=PROPERTY_DEFINITION_REPRESENTATION(#5841,#5766);
#5717=PROPERTY_DEFINITION_REPRESENTATION(#5842,#5767);
#5718=PROPERTY_DEFINITION_REPRESENTATION(#5843,#5768);
#5719=PROPERTY_DEFINITION_REPRESENTATION(#5844,#5769);
#5720=PROPERTY_DEFINITION_REPRESENTATION(#5845,#5770);
#5721=PROPERTY_DEFINITION_REPRESENTATION(#5846,#5771);
#5722=PROPERTY_DEFINITION_REPRESENTATION(#5847,#5772);
#5723=PROPERTY_DEFINITION_REPRESENTATION(#5848,#5773);
#5724=PROPERTY_DEFINITION_REPRESENTATION(#5849,#5774);
#5725=PROPERTY_DEFINITION_REPRESENTATION(#5850,#5775);
#5726=PROPERTY_DEFINITION_REPRESENTATION(#5851,#5776);
#5727=PROPERTY_DEFINITION_REPRESENTATION(#5852,#5777);
#5728=PROPERTY_DEFINITION_REPRESENTATION(#5853,#5778);
#5729=PROPERTY_DEFINITION_REPRESENTATION(#5854,#5779);
#5730=PROPERTY_DEFINITION_REPRESENTATION(#5855,#5780);
#5731=PROPERTY_DEFINITION_REPRESENTATION(#5856,#5781);
#5732=PROPERTY_DEFINITION_REPRESENTATION(#5857,#5782);
#5733=PROPERTY_DEFINITION_REPRESENTATION(#5858,#5783);
#5734=PROPERTY_DEFINITION_REPRESENTATION(#5859,#5784);
#5735=PROPERTY_DEFINITION_REPRESENTATION(#5860,#5785);
#5736=PROPERTY_DEFINITION_REPRESENTATION(#5861,#5786);
#5737=PROPERTY_DEFINITION_REPRESENTATION(#5862,#5787);
#5738=PROPERTY_DEFINITION_REPRESENTATION(#5863,#5788);
#5739=PROPERTY_DEFINITION_REPRESENTATION(#5864,#5789);
#5740=PROPERTY_DEFINITION_REPRESENTATION(#5865,#5790);
#5741=PROPERTY_DEFINITION_REPRESENTATION(#5866,#5791);
#5742=PROPERTY_DEFINITION_REPRESENTATION(#5867,#5792);
#5743=PROPERTY_DEFINITION_REPRESENTATION(#5868,#5793);
#5744=PROPERTY_DEFINITION_REPRESENTATION(#5869,#5794);
#5745=PROPERTY_DEFINITION_REPRESENTATION(#5870,#5795);
#5746=PROPERTY_DEFINITION_REPRESENTATION(#5871,#5796);
#5747=PROPERTY_DEFINITION_REPRESENTATION(#5872,#5797);
#5748=PROPERTY_DEFINITION_REPRESENTATION(#5873,#5798);
#5749=PROPERTY_DEFINITION_REPRESENTATION(#5874,#5799);
#5750=PROPERTY_DEFINITION_REPRESENTATION(#5875,#5800);
#5751=PROPERTY_DEFINITION_REPRESENTATION(#5876,#5801);
#5752=REPRESENTATION('material name',(#5802),#10794);
#5753=REPRESENTATION('density',(#5677),#10794);
#5754=REPRESENTATION('material name',(#5803),#10795);
#5755=REPRESENTATION('density',(#5678),#10795);
#5756=REPRESENTATION('material name',(#5804),#10796);
#5757=REPRESENTATION('density',(#5679),#10796);
#5758=REPRESENTATION('material name',(#5805),#10797);
#5759=REPRESENTATION('density',(#5680),#10797);
#5760=REPRESENTATION('material name',(#5806),#10798);
#5761=REPRESENTATION('density',(#5681),#10798);
#5762=REPRESENTATION('material name',(#5807),#10799);
#5763=REPRESENTATION('density',(#5682),#10799);
#5764=REPRESENTATION('material name',(#5808),#10800);
#5765=REPRESENTATION('density',(#5683),#10800);
#5766=REPRESENTATION('material name',(#5809),#10802);
#5767=REPRESENTATION('density',(#5684),#10802);
#5768=REPRESENTATION('material name',(#5810),#10803);
#5769=REPRESENTATION('density',(#5685),#10803);
#5770=REPRESENTATION('material name',(#5811),#10804);
#5771=REPRESENTATION('density',(#5686),#10804);
#5772=REPRESENTATION('material name',(#5812),#10805);
#5773=REPRESENTATION('density',(#5687),#10805);
#5774=REPRESENTATION('material name',(#5813),#10807);
#5775=REPRESENTATION('density',(#5688),#10807);
#5776=REPRESENTATION('material name',(#5814),#10808);
#5777=REPRESENTATION('density',(#5689),#10808);
#5778=REPRESENTATION('material name',(#5815),#10809);
#5779=REPRESENTATION('density',(#5690),#10809);
#5780=REPRESENTATION('material name',(#5816),#10810);
#5781=REPRESENTATION('density',(#5691),#10810);
#5782=REPRESENTATION('material name',(#5817),#10811);
#5783=REPRESENTATION('density',(#5692),#10811);
#5784=REPRESENTATION('material name',(#5818),#10812);
#5785=REPRESENTATION('density',(#5693),#10812);
#5786=REPRESENTATION('material name',(#5819),#10813);
#5787=REPRESENTATION('density',(#5694),#10813);
#5788=REPRESENTATION('material name',(#5820),#10814);
#5789=REPRESENTATION('density',(#5695),#10814);
#5790=REPRESENTATION('material name',(#5821),#10815);
#5791=REPRESENTATION('density',(#5696),#10815);
#5792=REPRESENTATION('material name',(#5822),#10816);
#5793=REPRESENTATION('density',(#5697),#10816);
#5794=REPRESENTATION('material name',(#5823),#10817);
#5795=REPRESENTATION('density',(#5698),#10817);
#5796=REPRESENTATION('material name',(#5824),#10818);
#5797=REPRESENTATION('density',(#5699),#10818);
#5798=REPRESENTATION('material name',(#5825),#10819);
#5799=REPRESENTATION('density',(#5700),#10819);
#5800=REPRESENTATION('material name',(#5826),#10820);
#5801=REPRESENTATION('density',(#5701),#10820);
#5802=DESCRIPTIVE_REPRESENTATION_ITEM('Steel','Steel');
#5803=DESCRIPTIVE_REPRESENTATION_ITEM('Steel','Steel');
#5804=DESCRIPTIVE_REPRESENTATION_ITEM('Steel','Steel');
#5805=DESCRIPTIVE_REPRESENTATION_ITEM('Steel','Steel');
#5806=DESCRIPTIVE_REPRESENTATION_ITEM('Steel','Steel');
#5807=DESCRIPTIVE_REPRESENTATION_ITEM('Steel','Steel');
#5808=DESCRIPTIVE_REPRESENTATION_ITEM('Steel','Steel');
#5809=DESCRIPTIVE_REPRESENTATION_ITEM('Steel','Steel');
#5810=DESCRIPTIVE_REPRESENTATION_ITEM('Steel','Steel');
#5811=DESCRIPTIVE_REPRESENTATION_ITEM('Steel','Steel');
#5812=DESCRIPTIVE_REPRESENTATION_ITEM('Steel','Steel');
#5813=DESCRIPTIVE_REPRESENTATION_ITEM('Steel','Steel');
#5814=DESCRIPTIVE_REPRESENTATION_ITEM('Steel','Steel');
#5815=DESCRIPTIVE_REPRESENTATION_ITEM('Steel','Steel');
#5816=DESCRIPTIVE_REPRESENTATION_ITEM('Steel','Steel');
#5817=DESCRIPTIVE_REPRESENTATION_ITEM('Steel','Steel');
#5818=DESCRIPTIVE_REPRESENTATION_ITEM('Steel','Steel');
#5819=DESCRIPTIVE_REPRESENTATION_ITEM('Steel','Steel');
#5820=DESCRIPTIVE_REPRESENTATION_ITEM('Steel','Steel');
#5821=DESCRIPTIVE_REPRESENTATION_ITEM('Steel','Steel');
#5822=DESCRIPTIVE_REPRESENTATION_ITEM('Steel','Steel');
#5823=DESCRIPTIVE_REPRESENTATION_ITEM('Steel','Steel');
#5824=DESCRIPTIVE_REPRESENTATION_ITEM('Steel','Steel');
#5825=DESCRIPTIVE_REPRESENTATION_ITEM('Steel','Steel');
#5826=DESCRIPTIVE_REPRESENTATION_ITEM('Steel','Steel');
#5827=PROPERTY_DEFINITION('material property','material name',#10956);
#5828=PROPERTY_DEFINITION('material property','density of part',#10956);
#5829=PROPERTY_DEFINITION('material property','material name',#10957);
#5830=PROPERTY_DEFINITION('material property','density of part',#10957);
#5831=PROPERTY_DEFINITION('material property','material name',#10958);
#5832=PROPERTY_DEFINITION('material property','density of part',#10958);
#5833=PROPERTY_DEFINITION('material property','material name',#10959);
#5834=PROPERTY_DEFINITION('material property','density of part',#10959);
#5835=PROPERTY_DEFINITION('material property','material name',#10960);
#5836=PROPERTY_DEFINITION('material property','density of part',#10960);
#5837=PROPERTY_DEFINITION('material property','material name',#10961);
#5838=PROPERTY_DEFINITION('material property','density of part',#10961);
#5839=PROPERTY_DEFINITION('material property','material name',#10962);
#5840=PROPERTY_DEFINITION('material property','density of part',#10962);
#5841=PROPERTY_DEFINITION('material property','material name',#10964);
#5842=PROPERTY_DEFINITION('material property','density of part',#10964);
#5843=PROPERTY_DEFINITION('material property','material name',#10965);
#5844=PROPERTY_DEFINITION('material property','density of part',#10965);
#5845=PROPERTY_DEFINITION('material property','material name',#10966);
#5846=PROPERTY_DEFINITION('material property','density of part',#10966);
#5847=PROPERTY_DEFINITION('material property','material name',#10967);
#5848=PROPERTY_DEFINITION('material property','density of part',#10967);
#5849=PROPERTY_DEFINITION('material property','material name',#10969);
#5850=PROPERTY_DEFINITION('material property','density of part',#10969);
#5851=PROPERTY_DEFINITION('material property','material name',#10970);
#5852=PROPERTY_DEFINITION('material property','density of part',#10970);
#5853=PROPERTY_DEFINITION('material property','material name',#10971);
#5854=PROPERTY_DEFINITION('material property','density of part',#10971);
#5855=PROPERTY_DEFINITION('material property','material name',#10972);
#5856=PROPERTY_DEFINITION('material property','density of part',#10972);
#5857=PROPERTY_DEFINITION('material property','material name',#10973);
#5858=PROPERTY_DEFINITION('material property','density of part',#10973);
#5859=PROPERTY_DEFINITION('material property','material name',#10974);
#5860=PROPERTY_DEFINITION('material property','density of part',#10974);
#5861=PROPERTY_DEFINITION('material property','material name',#10975);
#5862=PROPERTY_DEFINITION('material property','density of part',#10975);
#5863=PROPERTY_DEFINITION('material property','material name',#10976);
#5864=PROPERTY_DEFINITION('material property','density of part',#10976);
#5865=PROPERTY_DEFINITION('material property','material name',#10977);
#5866=PROPERTY_DEFINITION('material property','density of part',#10977);
#5867=PROPERTY_DEFINITION('material property','material name',#10978);
#5868=PROPERTY_DEFINITION('material property','density of part',#10978);
#5869=PROPERTY_DEFINITION('material property','material name',#10979);
#5870=PROPERTY_DEFINITION('material property','density of part',#10979);
#5871=PROPERTY_DEFINITION('material property','material name',#10980);
#5872=PROPERTY_DEFINITION('material property','density of part',#10980);
#5873=PROPERTY_DEFINITION('material property','material name',#10981);
#5874=PROPERTY_DEFINITION('material property','density of part',#10981);
#5875=PROPERTY_DEFINITION('material property','material name',#10982);
#5876=PROPERTY_DEFINITION('material property','density of part',#10982);
#5877=AXIS2_PLACEMENT_3D('',#8312,#6559,#6560);
#5878=AXIS2_PLACEMENT_3D('',#8313,#6561,#6562);
#5879=AXIS2_PLACEMENT_3D('',#8314,#6563,#6564);
#5880=AXIS2_PLACEMENT_3D('',#8315,#6565,#6566);
#5881=AXIS2_PLACEMENT_3D('',#8317,#6567,#6568);
#5882=AXIS2_PLACEMENT_3D('',#8320,#6570,#6571);
#5883=AXIS2_PLACEMENT_3D('',#8321,#6572,#6573);
#5884=AXIS2_PLACEMENT_3D('',#8323,#6574,#6575);
#5885=AXIS2_PLACEMENT_3D('',#8326,#6577,#6578);
#5886=AXIS2_PLACEMENT_3D('',#8327,#6579,#6580);
#5887=AXIS2_PLACEMENT_3D('',#8329,#6581,#6582);
#5888=AXIS2_PLACEMENT_3D('',#8332,#6584,#6585);
#5889=AXIS2_PLACEMENT_3D('',#8333,#6586,#6587);
#5890=AXIS2_PLACEMENT_3D('',#8335,#6588,#6589);
#5891=AXIS2_PLACEMENT_3D('',#8338,#6591,#6592);
#5892=AXIS2_PLACEMENT_3D('',#8339,#6593,#6594);
#5893=AXIS2_PLACEMENT_3D('',#8348,#6599,#6600);
#5894=AXIS2_PLACEMENT_3D('',#8354,#6604,#6605);
#5895=AXIS2_PLACEMENT_3D('',#8360,#6609,#6610);
#5896=AXIS2_PLACEMENT_3D('',#8363,#6613,#6614);
#5897=AXIS2_PLACEMENT_3D('',#8364,#6615,#6616);
#5898=AXIS2_PLACEMENT_3D('',#8365,#6617,#6618);
#5899=AXIS2_PLACEMENT_3D('',#8366,#6619,#6620);
#5900=AXIS2_PLACEMENT_3D('',#8375,#6625,#6626);
#5901=AXIS2_PLACEMENT_3D('',#8381,#6630,#6631);
#5902=AXIS2_PLACEMENT_3D('',#8387,#6635,#6636);
#5903=AXIS2_PLACEMENT_3D('',#8390,#6639,#6640);
#5904=AXIS2_PLACEMENT_3D('',#8391,#6641,#6642);
#5905=AXIS2_PLACEMENT_3D('',#8392,#6643,#6644);
#5906=AXIS2_PLACEMENT_3D('',#8393,#6645,#6646);
#5907=AXIS2_PLACEMENT_3D('',#8402,#6651,#6652);
#5908=AXIS2_PLACEMENT_3D('',#8408,#6656,#6657);
#5909=AXIS2_PLACEMENT_3D('',#8414,#6661,#6662);
#5910=AXIS2_PLACEMENT_3D('',#8417,#6665,#6666);
#5911=AXIS2_PLACEMENT_3D('',#8418,#6667,#6668);
#5912=AXIS2_PLACEMENT_3D('',#8419,#6669,#6670);
#5913=AXIS2_PLACEMENT_3D('',#8420,#6671,#6672);
#5914=AXIS2_PLACEMENT_3D('',#8422,#6673,#6674);
#5915=AXIS2_PLACEMENT_3D('',#8425,#6676,#6677);
#5916=AXIS2_PLACEMENT_3D('',#8426,#6678,#6679);
#5917=AXIS2_PLACEMENT_3D('',#8428,#6680,#6681);
#5918=AXIS2_PLACEMENT_3D('',#8431,#6683,#6684);
#5919=AXIS2_PLACEMENT_3D('',#8432,#6685,#6686);
#5920=AXIS2_PLACEMENT_3D('',#8433,#6687,#6688);
#5921=AXIS2_PLACEMENT_3D('',#8434,#6689,#6690);
#5922=AXIS2_PLACEMENT_3D('',#8435,#6691,#6692);
#5923=AXIS2_PLACEMENT_3D('',#8437,#6693,#6694);
#5924=AXIS2_PLACEMENT_3D('',#8440,#6696,#6697);
#5925=AXIS2_PLACEMENT_3D('',#8441,#6698,#6699);
#5926=AXIS2_PLACEMENT_3D('',#8443,#6700,#6701);
#5927=AXIS2_PLACEMENT_3D('',#8446,#6703,#6704);
#5928=AXIS2_PLACEMENT_3D('',#8447,#6705,#6706);
#5929=AXIS2_PLACEMENT_3D('',#8448,#6707,#6708);
#5930=AXIS2_PLACEMENT_3D('',#8449,#6709,#6710);
#5931=AXIS2_PLACEMENT_3D('',#8450,#6711,#6712);
#5932=AXIS2_PLACEMENT_3D('',#8452,#6713,#6714);
#5933=AXIS2_PLACEMENT_3D('',#8455,#6716,#6717);
#5934=AXIS2_PLACEMENT_3D('',#8456,#6718,#6719);
#5935=AXIS2_PLACEMENT_3D('',#8458,#6720,#6721);
#5936=AXIS2_PLACEMENT_3D('',#8461,#6723,#6724);
#5937=AXIS2_PLACEMENT_3D('',#8462,#6725,#6726);
#5938=AXIS2_PLACEMENT_3D('',#8463,#6727,#6728);
#5939=AXIS2_PLACEMENT_3D('',#8464,#6729,#6730);
#5940=AXIS2_PLACEMENT_3D('',#8465,#6731,#6732);
#5941=AXIS2_PLACEMENT_3D('',#8467,#6733,#6734);
#5942=AXIS2_PLACEMENT_3D('',#8470,#6736,#6737);
#5943=AXIS2_PLACEMENT_3D('',#8471,#6738,#6739);
#5944=AXIS2_PLACEMENT_3D('',#8473,#6740,#6741);
#5945=AXIS2_PLACEMENT_3D('',#8476,#6743,#6744);
#5946=AXIS2_PLACEMENT_3D('',#8477,#6745,#6746);
#5947=AXIS2_PLACEMENT_3D('',#8478,#6747,#6748);
#5948=AXIS2_PLACEMENT_3D('',#8479,#6749,#6750);
#5949=AXIS2_PLACEMENT_3D('',#8480,#6751,#6752);
#5950=AXIS2_PLACEMENT_3D('',#8481,#6753,#6754);
#5951=AXIS2_PLACEMENT_3D('',#8483,#6755,#6756);
#5952=AXIS2_PLACEMENT_3D('',#8486,#6758,#6759);
#5953=AXIS2_PLACEMENT_3D('',#8487,#6760,#6761);
#5954=AXIS2_PLACEMENT_3D('',#8489,#6762,#6763);
#5955=AXIS2_PLACEMENT_3D('',#8492,#6765,#6766);
#5956=AXIS2_PLACEMENT_3D('',#8493,#6767,#6768);
#5957=AXIS2_PLACEMENT_3D('',#8496,#6769,#6770);
#5958=AXIS2_PLACEMENT_3D('',#8497,#6771,#6772);
#5959=AXIS2_PLACEMENT_3D('',#8503,#6775,#6776);
#5960=AXIS2_PLACEMENT_3D('',#8504,#6777,#6778);
#5961=AXIS2_PLACEMENT_3D('',#8509,#6780,#6781);
#5962=AXIS2_PLACEMENT_3D('',#8511,#6783,#6784);
#5963=AXIS2_PLACEMENT_3D('',#8516,#6786,#6787);
#5964=AXIS2_PLACEMENT_3D('',#8518,#6789,#6790);
#5965=AXIS2_PLACEMENT_3D('',#8521,#6793,#6794);
#5966=AXIS2_PLACEMENT_3D('',#8527,#6797,#6798);
#5967=AXIS2_PLACEMENT_3D('',#8528,#6799,#6800);
#5968=AXIS2_PLACEMENT_3D('',#8531,#6803,#6804);
#5969=AXIS2_PLACEMENT_3D('',#8541,#6809,#6810);
#5970=AXIS2_PLACEMENT_3D('',#8543,#6811,#6812);
#5971=AXIS2_PLACEMENT_3D('',#8554,#6819,#6820);
#5972=AXIS2_PLACEMENT_3D('',#8555,#6821,#6822);
#5973=AXIS2_PLACEMENT_3D('',#8556,#6823,#6824);
#5974=AXIS2_PLACEMENT_3D('',#8557,#6825,#6826);
#5975=AXIS2_PLACEMENT_3D('',#8558,#6827,#6828);
#5976=AXIS2_PLACEMENT_3D('',#8559,#6829,#6830);
#5977=AXIS2_PLACEMENT_3D('',#8568,#6835,#6836);
#5978=AXIS2_PLACEMENT_3D('',#8574,#6840,#6841);
#5979=AXIS2_PLACEMENT_3D('',#8580,#6845,#6846);
#5980=AXIS2_PLACEMENT_3D('',#8583,#6849,#6850);
#5981=AXIS2_PLACEMENT_3D('',#8584,#6851,#6852);
#5982=AXIS2_PLACEMENT_3D('',#8586,#6853,#6854);
#5983=AXIS2_PLACEMENT_3D('',#8588,#6856,#6857);
#5984=AXIS2_PLACEMENT_3D('',#8590,#6858,#6859);
#5985=AXIS2_PLACEMENT_3D('',#8592,#6861,#6862);
#5986=AXIS2_PLACEMENT_3D('',#8598,#6866,#6867);
#5987=AXIS2_PLACEMENT_3D('',#8602,#6870,#6871);
#5988=AXIS2_PLACEMENT_3D('',#8606,#6874,#6875);
#5989=AXIS2_PLACEMENT_3D('',#8608,#6877,#6878);
#5990=AXIS2_PLACEMENT_3D('',#8609,#6879,#6880);
#5991=AXIS2_PLACEMENT_3D('',#8610,#6881,#6882);
#5992=AXIS2_PLACEMENT_3D('',#8612,#6883,#6884);
#5993=AXIS2_PLACEMENT_3D('',#8615,#6886,#6887);
#5994=AXIS2_PLACEMENT_3D('',#8616,#6888,#6889);
#5995=AXIS2_PLACEMENT_3D('',#8618,#6890,#6891);
#5996=AXIS2_PLACEMENT_3D('',#8619,#6892,#6893);
#5997=AXIS2_PLACEMENT_3D('',#8622,#6894,#6895);
#5998=AXIS2_PLACEMENT_3D('',#8624,#6896,#6897);
#5999=AXIS2_PLACEMENT_3D('',#8625,#6898,#6899);
#6000=AXIS2_PLACEMENT_3D('',#8626,#6900,#6901);
#6001=AXIS2_PLACEMENT_3D('',#8704,#6903,#6904);
#6002=AXIS2_PLACEMENT_3D('',#8782,#6906,#6907);
#6003=AXIS2_PLACEMENT_3D('',#8784,#6908,#6909);
#6004=AXIS2_PLACEMENT_3D('',#8787,#6911,#6912);
#6005=AXIS2_PLACEMENT_3D('',#8952,#6913,#6914);
#6006=AXIS2_PLACEMENT_3D('',#8989,#6916,#6917);
#6007=AXIS2_PLACEMENT_3D('',#9026,#6919,#6920);
#6008=AXIS2_PLACEMENT_3D('',#9063,#6922,#6923);
#6009=AXIS2_PLACEMENT_3D('',#9100,#6925,#6926);
#6010=AXIS2_PLACEMENT_3D('',#9102,#6927,#6928);
#6011=AXIS2_PLACEMENT_3D('',#9103,#6929,#6930);
#6012=AXIS2_PLACEMENT_3D('',#9105,#6931,#6932);
#6013=AXIS2_PLACEMENT_3D('',#9106,#6933,#6934);
#6014=AXIS2_PLACEMENT_3D('',#9108,#6935,#6936);
#6015=AXIS2_PLACEMENT_3D('',#9110,#6938,#6939);
#6016=AXIS2_PLACEMENT_3D('',#9112,#6940,#6941);
#6017=AXIS2_PLACEMENT_3D('',#9113,#6942,#6943);
#6018=AXIS2_PLACEMENT_3D('',#9115,#6945,#6946);
#6019=AXIS2_PLACEMENT_3D('',#9116,#6947,#6948);
#6020=AXIS2_PLACEMENT_3D('',#9117,#6949,#6950);
#6021=AXIS2_PLACEMENT_3D('',#9118,#6951,#6952);
#6022=AXIS2_PLACEMENT_3D('',#9120,#6953,#6954);
#6023=AXIS2_PLACEMENT_3D('',#9123,#6956,#6957);
#6024=AXIS2_PLACEMENT_3D('',#9124,#6958,#6959);
#6025=AXIS2_PLACEMENT_3D('',#9126,#6960,#6961);
#6026=AXIS2_PLACEMENT_3D('',#9129,#6963,#6964);
#6027=AXIS2_PLACEMENT_3D('',#9130,#6965,#6966);
#6028=AXIS2_PLACEMENT_3D('',#9131,#6967,#6968);
#6029=AXIS2_PLACEMENT_3D('',#9132,#6969,#6970);
#6030=AXIS2_PLACEMENT_3D('',#9133,#6971,#6972);
#6031=AXIS2_PLACEMENT_3D('',#9142,#6977,#6978);
#6032=AXIS2_PLACEMENT_3D('',#9148,#6982,#6983);
#6033=AXIS2_PLACEMENT_3D('',#9154,#6987,#6988);
#6034=AXIS2_PLACEMENT_3D('',#9160,#6992,#6993);
#6035=AXIS2_PLACEMENT_3D('',#9166,#6997,#6998);
#6036=AXIS2_PLACEMENT_3D('',#9169,#7001,#7002);
#6037=AXIS2_PLACEMENT_3D('',#9170,#7003,#7004);
#6038=AXIS2_PLACEMENT_3D('',#9171,#7005,#7006);
#6039=AXIS2_PLACEMENT_3D('',#9173,#7007,#7008);
#6040=AXIS2_PLACEMENT_3D('',#9174,#7009,#7010);
#6041=AXIS2_PLACEMENT_3D('',#9176,#7011,#7012);
#6042=AXIS2_PLACEMENT_3D('',#9177,#7013,#7014);
#6043=AXIS2_PLACEMENT_3D('',#9179,#7015,#7016);
#6044=AXIS2_PLACEMENT_3D('',#9181,#7018,#7019);
#6045=AXIS2_PLACEMENT_3D('',#9183,#7020,#7021);
#6046=AXIS2_PLACEMENT_3D('',#9185,#7023,#7024);
#6047=AXIS2_PLACEMENT_3D('',#9187,#7025,#7026);
#6048=AXIS2_PLACEMENT_3D('',#9189,#7028,#7029);
#6049=AXIS2_PLACEMENT_3D('',#9191,#7030,#7031);
#6050=AXIS2_PLACEMENT_3D('',#9192,#7032,#7033);
#6051=AXIS2_PLACEMENT_3D('',#9194,#7034,#7035);
#6052=AXIS2_PLACEMENT_3D('',#9196,#7037,#7038);
#6053=AXIS2_PLACEMENT_3D('',#9198,#7040,#7041);
#6054=AXIS2_PLACEMENT_3D('',#9199,#7042,#7043);
#6055=AXIS2_PLACEMENT_3D('',#9200,#7044,#7045);
#6056=AXIS2_PLACEMENT_3D('',#9201,#7046,#7047);
#6057=AXIS2_PLACEMENT_3D('',#9202,#7048,#7049);
#6058=AXIS2_PLACEMENT_3D('',#9203,#7050,#7051);
#6059=AXIS2_PLACEMENT_3D('',#9204,#7052,#7053);
#6060=AXIS2_PLACEMENT_3D('',#9205,#7054,#7055);
#6061=AXIS2_PLACEMENT_3D('',#9206,#7056,#7057);
#6062=AXIS2_PLACEMENT_3D('',#9207,#7058,#7059);
#6063=AXIS2_PLACEMENT_3D('',#9208,#7060,#7061);
#6064=AXIS2_PLACEMENT_3D('',#9209,#7062,#7063);
#6065=AXIS2_PLACEMENT_3D('',#9210,#7064,#7065);
#6066=AXIS2_PLACEMENT_3D('',#9211,#7066,#7067);
#6067=AXIS2_PLACEMENT_3D('',#9212,#7068,#7069);
#6068=AXIS2_PLACEMENT_3D('',#9213,#7070,#7071);
#6069=AXIS2_PLACEMENT_3D('',#9214,#7072,#7073);
#6070=AXIS2_PLACEMENT_3D('',#9215,#7074,#7075);
#6071=AXIS2_PLACEMENT_3D('',#9216,#7076,#7077);
#6072=AXIS2_PLACEMENT_3D('',#9217,#7078,#7079);
#6073=AXIS2_PLACEMENT_3D('',#9226,#7084,#7085);
#6074=AXIS2_PLACEMENT_3D('',#9228,#7086,#7087);
#6075=AXIS2_PLACEMENT_3D('',#9232,#7090,#7091);
#6076=AXIS2_PLACEMENT_3D('',#9238,#7095,#7096);
#6077=AXIS2_PLACEMENT_3D('',#9240,#7098,#7099);
#6078=AXIS2_PLACEMENT_3D('',#9241,#7100,#7101);
#6079=AXIS2_PLACEMENT_3D('',#9242,#7102,#7103);
#6080=AXIS2_PLACEMENT_3D('',#9244,#7104,#7105);
#6081=AXIS2_PLACEMENT_3D('',#9247,#7107,#7108);
#6082=AXIS2_PLACEMENT_3D('',#9248,#7109,#7110);
#6083=AXIS2_PLACEMENT_3D('',#9249,#7111,#7112);
#6084=AXIS2_PLACEMENT_3D('',#9251,#7113,#7114);
#6085=AXIS2_PLACEMENT_3D('',#9254,#7116,#7117);
#6086=AXIS2_PLACEMENT_3D('',#9255,#7118,#7119);
#6087=AXIS2_PLACEMENT_3D('',#9256,#7120,#7121);
#6088=AXIS2_PLACEMENT_3D('',#9265,#7126,#7127);
#6089=AXIS2_PLACEMENT_3D('',#9267,#7128,#7129);
#6090=AXIS2_PLACEMENT_3D('',#9271,#7132,#7133);
#6091=AXIS2_PLACEMENT_3D('',#9277,#7137,#7138);
#6092=AXIS2_PLACEMENT_3D('',#9279,#7140,#7141);
#6093=AXIS2_PLACEMENT_3D('',#9280,#7142,#7143);
#6094=AXIS2_PLACEMENT_3D('',#9281,#7144,#7145);
#6095=AXIS2_PLACEMENT_3D('',#9290,#7150,#7151);
#6096=AXIS2_PLACEMENT_3D('',#9292,#7152,#7153);
#6097=AXIS2_PLACEMENT_3D('',#9296,#7156,#7157);
#6098=AXIS2_PLACEMENT_3D('',#9302,#7161,#7162);
#6099=AXIS2_PLACEMENT_3D('',#9304,#7164,#7165);
#6100=AXIS2_PLACEMENT_3D('',#9305,#7166,#7167);
#6101=AXIS2_PLACEMENT_3D('',#9306,#7168,#7169);
#6102=AXIS2_PLACEMENT_3D('',#9308,#7170,#7171);
#6103=AXIS2_PLACEMENT_3D('',#9311,#7173,#7174);
#6104=AXIS2_PLACEMENT_3D('',#9312,#7175,#7176);
#6105=AXIS2_PLACEMENT_3D('',#9313,#7177,#7178);
#6106=AXIS2_PLACEMENT_3D('',#9315,#7179,#7180);
#6107=AXIS2_PLACEMENT_3D('',#9318,#7182,#7183);
#6108=AXIS2_PLACEMENT_3D('',#9319,#7184,#7185);
#6109=AXIS2_PLACEMENT_3D('',#9320,#7186,#7187);
#6110=AXIS2_PLACEMENT_3D('',#9322,#7188,#7189);
#6111=AXIS2_PLACEMENT_3D('',#9325,#7191,#7192);
#6112=AXIS2_PLACEMENT_3D('',#9326,#7193,#7194);
#6113=AXIS2_PLACEMENT_3D('',#9327,#7195,#7196);
#6114=AXIS2_PLACEMENT_3D('',#9328,#7197,#7198);
#6115=AXIS2_PLACEMENT_3D('',#9329,#7199,#7200);
#6116=AXIS2_PLACEMENT_3D('',#9331,#7201,#7202);
#6117=AXIS2_PLACEMENT_3D('',#9334,#7204,#7205);
#6118=AXIS2_PLACEMENT_3D('',#9335,#7206,#7207);
#6119=AXIS2_PLACEMENT_3D('',#9337,#7208,#7209);
#6120=AXIS2_PLACEMENT_3D('',#9340,#7211,#7212);
#6121=AXIS2_PLACEMENT_3D('',#9341,#7213,#7214);
#6122=AXIS2_PLACEMENT_3D('',#9342,#7215,#7216);
#6123=AXIS2_PLACEMENT_3D('',#9343,#7217,#7218);
#6124=AXIS2_PLACEMENT_3D('',#9344,#7219,#7220);
#6125=AXIS2_PLACEMENT_3D('',#9346,#7221,#7222);
#6126=AXIS2_PLACEMENT_3D('',#9349,#7224,#7225);
#6127=AXIS2_PLACEMENT_3D('',#9350,#7226,#7227);
#6128=AXIS2_PLACEMENT_3D('',#9352,#7228,#7229);
#6129=AXIS2_PLACEMENT_3D('',#9355,#7231,#7232);
#6130=AXIS2_PLACEMENT_3D('',#9356,#7233,#7234);
#6131=AXIS2_PLACEMENT_3D('',#9357,#7235,#7236);
#6132=AXIS2_PLACEMENT_3D('',#9358,#7237,#7238);
#6133=AXIS2_PLACEMENT_3D('',#9359,#7239,#7240);
#6134=AXIS2_PLACEMENT_3D('',#9361,#7241,#7242);
#6135=AXIS2_PLACEMENT_3D('',#9364,#7244,#7245);
#6136=AXIS2_PLACEMENT_3D('',#9365,#7246,#7247);
#6137=AXIS2_PLACEMENT_3D('',#9367,#7248,#7249);
#6138=AXIS2_PLACEMENT_3D('',#9370,#7251,#7252);
#6139=AXIS2_PLACEMENT_3D('',#9371,#7253,#7254);
#6140=AXIS2_PLACEMENT_3D('',#9372,#7255,#7256);
#6141=AXIS2_PLACEMENT_3D('',#9373,#7257,#7258);
#6142=AXIS2_PLACEMENT_3D('',#9374,#7259,#7260);
#6143=AXIS2_PLACEMENT_3D('',#9376,#7261,#7262);
#6144=AXIS2_PLACEMENT_3D('',#9379,#7264,#7265);
#6145=AXIS2_PLACEMENT_3D('',#9380,#7266,#7267);
#6146=AXIS2_PLACEMENT_3D('',#9382,#7268,#7269);
#6147=AXIS2_PLACEMENT_3D('',#9385,#7271,#7272);
#6148=AXIS2_PLACEMENT_3D('',#9386,#7273,#7274);
#6149=AXIS2_PLACEMENT_3D('',#9387,#7275,#7276);
#6150=AXIS2_PLACEMENT_3D('',#9388,#7277,#7278);
#6151=AXIS2_PLACEMENT_3D('',#9389,#7279,#7280);
#6152=AXIS2_PLACEMENT_3D('',#9391,#7281,#7282);
#6153=AXIS2_PLACEMENT_3D('',#9394,#7284,#7285);
#6154=AXIS2_PLACEMENT_3D('',#9395,#7286,#7287);
#6155=AXIS2_PLACEMENT_3D('',#9397,#7288,#7289);
#6156=AXIS2_PLACEMENT_3D('',#9400,#7291,#7292);
#6157=AXIS2_PLACEMENT_3D('',#9401,#7293,#7294);
#6158=AXIS2_PLACEMENT_3D('',#9402,#7295,#7296);
#6159=AXIS2_PLACEMENT_3D('',#9403,#7297,#7298);
#6160=AXIS2_PLACEMENT_3D('',#9404,#7299,#7300);
#6161=AXIS2_PLACEMENT_3D('',#9408,#7302,#7303);
#6162=AXIS2_PLACEMENT_3D('',#9409,#7304,#7305);
#6163=AXIS2_PLACEMENT_3D('',#9422,#7306,#7307);
#6164=AXIS2_PLACEMENT_3D('',#9463,#7309,#7310);
#6165=AXIS2_PLACEMENT_3D('',#9474,#7311,#7312);
#6166=AXIS2_PLACEMENT_3D('',#9476,#7314,#7315);
#6167=AXIS2_PLACEMENT_3D('',#9485,#7320,#7321);
#6168=AXIS2_PLACEMENT_3D('',#9491,#7325,#7326);
#6169=AXIS2_PLACEMENT_3D('',#9497,#7330,#7331);
#6170=AXIS2_PLACEMENT_3D('',#9499,#7332,#7333);
#6171=AXIS2_PLACEMENT_3D('',#9500,#7334,#7335);
#6172=AXIS2_PLACEMENT_3D('',#9501,#7336,#7337);
#6173=AXIS2_PLACEMENT_3D('',#9502,#7338,#7339);
#6174=AXIS2_PLACEMENT_3D('',#9503,#7340,#7341);
#6175=AXIS2_PLACEMENT_3D('',#9506,#7343,#7344);
#6176=AXIS2_PLACEMENT_3D('',#9507,#7345,#7346);
#6177=AXIS2_PLACEMENT_3D('',#9508,#7347,#7348);
#6178=AXIS2_PLACEMENT_3D('',#9509,#7349,#7350);
#6179=AXIS2_PLACEMENT_3D('',#9513,#7352,#7353);
#6180=AXIS2_PLACEMENT_3D('',#9514,#7354,#7355);
#6181=AXIS2_PLACEMENT_3D('',#9531,#7356,#7357);
#6182=AXIS2_PLACEMENT_3D('',#9572,#7359,#7360);
#6183=AXIS2_PLACEMENT_3D('',#9587,#7361,#7362);
#6184=AXIS2_PLACEMENT_3D('',#9589,#7364,#7365);
#6185=AXIS2_PLACEMENT_3D('',#9591,#7366,#7367);
#6186=AXIS2_PLACEMENT_3D('',#9594,#7369,#7370);
#6187=AXIS2_PLACEMENT_3D('',#9595,#7371,#7372);
#6188=AXIS2_PLACEMENT_3D('',#9597,#7373,#7374);
#6189=AXIS2_PLACEMENT_3D('',#9600,#7376,#7377);
#6190=AXIS2_PLACEMENT_3D('',#9601,#7378,#7379);
#6191=AXIS2_PLACEMENT_3D('',#9602,#7380,#7381);
#6192=AXIS2_PLACEMENT_3D('',#9603,#7382,#7383);
#6193=AXIS2_PLACEMENT_3D('',#9604,#7384,#7385);
#6194=AXIS2_PLACEMENT_3D('',#9608,#7387,#7388);
#6195=AXIS2_PLACEMENT_3D('',#9609,#7389,#7390);
#6196=AXIS2_PLACEMENT_3D('',#9626,#7391,#7392);
#6197=AXIS2_PLACEMENT_3D('',#9667,#7394,#7395);
#6198=AXIS2_PLACEMENT_3D('',#9682,#7396,#7397);
#6199=AXIS2_PLACEMENT_3D('',#9684,#7399,#7400);
#6200=AXIS2_PLACEMENT_3D('',#9686,#7401,#7402);
#6201=AXIS2_PLACEMENT_3D('',#9689,#7404,#7405);
#6202=AXIS2_PLACEMENT_3D('',#9690,#7406,#7407);
#6203=AXIS2_PLACEMENT_3D('',#9692,#7408,#7409);
#6204=AXIS2_PLACEMENT_3D('',#9695,#7411,#7412);
#6205=AXIS2_PLACEMENT_3D('',#9696,#7413,#7414);
#6206=AXIS2_PLACEMENT_3D('',#9697,#7415,#7416);
#6207=AXIS2_PLACEMENT_3D('',#9698,#7417,#7418);
#6208=AXIS2_PLACEMENT_3D('',#9699,#7419,#7420);
#6209=AXIS2_PLACEMENT_3D('',#9708,#7425,#7426);
#6210=AXIS2_PLACEMENT_3D('',#9715,#7430,#7431);
#6211=AXIS2_PLACEMENT_3D('',#9716,#7432,#7433);
#6212=AXIS2_PLACEMENT_3D('',#9722,#7437,#7438);
#6213=AXIS2_PLACEMENT_3D('',#9724,#7439,#7440);
#6214=AXIS2_PLACEMENT_3D('',#9725,#7441,#7442);
#6215=AXIS2_PLACEMENT_3D('',#9726,#7443,#7444);
#6216=AXIS2_PLACEMENT_3D('',#9727,#7445,#7446);
#6217=AXIS2_PLACEMENT_3D('',#9842,#7447,#7448);
#6218=AXIS2_PLACEMENT_3D('',#9885,#7450,#7451);
#6219=AXIS2_PLACEMENT_3D('',#9928,#7453,#7454);
#6220=AXIS2_PLACEMENT_3D('',#9930,#7455,#7456);
#6221=AXIS2_PLACEMENT_3D('',#9934,#7459,#7460);
#6222=AXIS2_PLACEMENT_3D('',#10017,#7461,#7462);
#6223=AXIS2_PLACEMENT_3D('',#10019,#7464,#7465);
#6224=AXIS2_PLACEMENT_3D('',#10021,#7467,#7468);
#6225=AXIS2_PLACEMENT_3D('',#10022,#7469,#7470);
#6226=AXIS2_PLACEMENT_3D('',#10024,#7471,#7472);
#6227=AXIS2_PLACEMENT_3D('',#10027,#7473,#7474);
#6228=AXIS2_PLACEMENT_3D('',#10029,#7475,#7476);
#6229=AXIS2_PLACEMENT_3D('',#10031,#7477,#7478);
#6230=AXIS2_PLACEMENT_3D('',#10033,#7479,#7480);
#6231=AXIS2_PLACEMENT_3D('',#10035,#7481,#7482);
#6232=AXIS2_PLACEMENT_3D('',#10037,#7483,#7484);
#6233=AXIS2_PLACEMENT_3D('',#10039,#7485,#7486);
#6234=AXIS2_PLACEMENT_3D('',#10041,#7487,#7488);
#6235=AXIS2_PLACEMENT_3D('',#10043,#7489,#7490);
#6236=AXIS2_PLACEMENT_3D('',#10045,#7491,#7492);
#6237=AXIS2_PLACEMENT_3D('',#10047,#7493,#7494);
#6238=AXIS2_PLACEMENT_3D('',#10049,#7495,#7496);
#6239=AXIS2_PLACEMENT_3D('',#10051,#7497,#7498);
#6240=AXIS2_PLACEMENT_3D('',#10053,#7499,#7500);
#6241=AXIS2_PLACEMENT_3D('',#10055,#7501,#7502);
#6242=AXIS2_PLACEMENT_3D('',#10057,#7503,#7504);
#6243=AXIS2_PLACEMENT_3D('',#10059,#7505,#7506);
#6244=AXIS2_PLACEMENT_3D('',#10061,#7507,#7508);
#6245=AXIS2_PLACEMENT_3D('',#10063,#7509,#7510);
#6246=AXIS2_PLACEMENT_3D('',#10065,#7511,#7512);
#6247=AXIS2_PLACEMENT_3D('',#10067,#7513,#7514);
#6248=AXIS2_PLACEMENT_3D('',#10069,#7515,#7516);
#6249=AXIS2_PLACEMENT_3D('',#10071,#7517,#7518);
#6250=AXIS2_PLACEMENT_3D('',#10073,#7519,#7520);
#6251=AXIS2_PLACEMENT_3D('',#10075,#7521,#7522);
#6252=AXIS2_PLACEMENT_3D('',#10077,#7523,#7524);
#6253=AXIS2_PLACEMENT_3D('',#10079,#7525,#7526);
#6254=AXIS2_PLACEMENT_3D('',#10081,#7527,#7528);
#6255=AXIS2_PLACEMENT_3D('',#10083,#7529,#7530);
#6256=AXIS2_PLACEMENT_3D('',#10085,#7531,#7532);
#6257=AXIS2_PLACEMENT_3D('',#10087,#7533,#7534);
#6258=AXIS2_PLACEMENT_3D('',#10089,#7535,#7536);
#6259=AXIS2_PLACEMENT_3D('',#10091,#7537,#7538);
#6260=AXIS2_PLACEMENT_3D('',#10093,#7539,#7540);
#6261=AXIS2_PLACEMENT_3D('',#10095,#7541,#7542);
#6262=AXIS2_PLACEMENT_3D('',#10097,#7543,#7544);
#6263=AXIS2_PLACEMENT_3D('',#10099,#7545,#7546);
#6264=AXIS2_PLACEMENT_3D('',#10101,#7547,#7548);
#6265=AXIS2_PLACEMENT_3D('',#10103,#7549,#7550);
#6266=AXIS2_PLACEMENT_3D('',#10105,#7551,#7552);
#6267=AXIS2_PLACEMENT_3D('',#10107,#7553,#7554);
#6268=AXIS2_PLACEMENT_3D('',#10109,#7555,#7556);
#6269=AXIS2_PLACEMENT_3D('',#10111,#7557,#7558);
#6270=AXIS2_PLACEMENT_3D('',#10113,#7559,#7560);
#6271=AXIS2_PLACEMENT_3D('',#10115,#7561,#7562);
#6272=AXIS2_PLACEMENT_3D('',#10117,#7563,#7564);
#6273=AXIS2_PLACEMENT_3D('',#10119,#7565,#7566);
#6274=AXIS2_PLACEMENT_3D('',#10121,#7567,#7568);
#6275=AXIS2_PLACEMENT_3D('',#10123,#7569,#7570);
#6276=AXIS2_PLACEMENT_3D('',#10125,#7571,#7572);
#6277=AXIS2_PLACEMENT_3D('',#10127,#7573,#7574);
#6278=AXIS2_PLACEMENT_3D('',#10129,#7575,#7576);
#6279=AXIS2_PLACEMENT_3D('',#10131,#7577,#7578);
#6280=AXIS2_PLACEMENT_3D('',#10133,#7579,#7580);
#6281=AXIS2_PLACEMENT_3D('',#10135,#7581,#7582);
#6282=AXIS2_PLACEMENT_3D('',#10137,#7583,#7584);
#6283=AXIS2_PLACEMENT_3D('',#10139,#7585,#7586);
#6284=AXIS2_PLACEMENT_3D('',#10141,#7587,#7588);
#6285=AXIS2_PLACEMENT_3D('',#10143,#7589,#7590);
#6286=AXIS2_PLACEMENT_3D('',#10145,#7591,#7592);
#6287=AXIS2_PLACEMENT_3D('',#10147,#7593,#7594);
#6288=AXIS2_PLACEMENT_3D('',#10149,#7595,#7596);
#6289=AXIS2_PLACEMENT_3D('',#10151,#7597,#7598);
#6290=AXIS2_PLACEMENT_3D('',#10153,#7599,#7600);
#6291=AXIS2_PLACEMENT_3D('',#10155,#7601,#7602);
#6292=AXIS2_PLACEMENT_3D('',#10157,#7603,#7604);
#6293=AXIS2_PLACEMENT_3D('',#10159,#7605,#7606);
#6294=AXIS2_PLACEMENT_3D('',#10161,#7607,#7608);
#6295=AXIS2_PLACEMENT_3D('',#10163,#7609,#7610);
#6296=AXIS2_PLACEMENT_3D('',#10165,#7611,#7612);
#6297=AXIS2_PLACEMENT_3D('',#10167,#7613,#7614);
#6298=AXIS2_PLACEMENT_3D('',#10169,#7615,#7616);
#6299=AXIS2_PLACEMENT_3D('',#10171,#7617,#7618);
#6300=AXIS2_PLACEMENT_3D('',#10173,#7619,#7620);
#6301=AXIS2_PLACEMENT_3D('',#10175,#7621,#7622);
#6302=AXIS2_PLACEMENT_3D('',#10177,#7623,#7624);
#6303=AXIS2_PLACEMENT_3D('',#10179,#7625,#7626);
#6304=AXIS2_PLACEMENT_3D('',#10181,#7627,#7628);
#6305=AXIS2_PLACEMENT_3D('',#10183,#7629,#7630);
#6306=AXIS2_PLACEMENT_3D('',#10184,#7631,#7632);
#6307=AXIS2_PLACEMENT_3D('',#10185,#7633,#7634);
#6308=AXIS2_PLACEMENT_3D('',#10187,#7635,#7636);
#6309=AXIS2_PLACEMENT_3D('',#10189,#7638,#7639);
#6310=AXIS2_PLACEMENT_3D('',#10190,#7640,#7641);
#6311=AXIS2_PLACEMENT_3D('',#10192,#7642,#7643);
#6312=AXIS2_PLACEMENT_3D('',#10195,#7644,#7645);
#6313=AXIS2_PLACEMENT_3D('',#10197,#7646,#7647);
#6314=AXIS2_PLACEMENT_3D('',#10199,#7648,#7649);
#6315=AXIS2_PLACEMENT_3D('',#10201,#7650,#7651);
#6316=AXIS2_PLACEMENT_3D('',#10203,#7652,#7653);
#6317=AXIS2_PLACEMENT_3D('',#10205,#7654,#7655);
#6318=AXIS2_PLACEMENT_3D('',#10207,#7656,#7657);
#6319=AXIS2_PLACEMENT_3D('',#10209,#7658,#7659);
#6320=AXIS2_PLACEMENT_3D('',#10211,#7660,#7661);
#6321=AXIS2_PLACEMENT_3D('',#10213,#7662,#7663);
#6322=AXIS2_PLACEMENT_3D('',#10215,#7664,#7665);
#6323=AXIS2_PLACEMENT_3D('',#10217,#7666,#7667);
#6324=AXIS2_PLACEMENT_3D('',#10219,#7668,#7669);
#6325=AXIS2_PLACEMENT_3D('',#10221,#7670,#7671);
#6326=AXIS2_PLACEMENT_3D('',#10223,#7672,#7673);
#6327=AXIS2_PLACEMENT_3D('',#10225,#7674,#7675);
#6328=AXIS2_PLACEMENT_3D('',#10227,#7676,#7677);
#6329=AXIS2_PLACEMENT_3D('',#10229,#7678,#7679);
#6330=AXIS2_PLACEMENT_3D('',#10231,#7680,#7681);
#6331=AXIS2_PLACEMENT_3D('',#10233,#7682,#7683);
#6332=AXIS2_PLACEMENT_3D('',#10235,#7684,#7685);
#6333=AXIS2_PLACEMENT_3D('',#10237,#7686,#7687);
#6334=AXIS2_PLACEMENT_3D('',#10239,#7688,#7689);
#6335=AXIS2_PLACEMENT_3D('',#10241,#7690,#7691);
#6336=AXIS2_PLACEMENT_3D('',#10243,#7692,#7693);
#6337=AXIS2_PLACEMENT_3D('',#10245,#7694,#7695);
#6338=AXIS2_PLACEMENT_3D('',#10247,#7696,#7697);
#6339=AXIS2_PLACEMENT_3D('',#10249,#7698,#7699);
#6340=AXIS2_PLACEMENT_3D('',#10251,#7700,#7701);
#6341=AXIS2_PLACEMENT_3D('',#10253,#7702,#7703);
#6342=AXIS2_PLACEMENT_3D('',#10255,#7704,#7705);
#6343=AXIS2_PLACEMENT_3D('',#10257,#7706,#7707);
#6344=AXIS2_PLACEMENT_3D('',#10259,#7708,#7709);
#6345=AXIS2_PLACEMENT_3D('',#10261,#7710,#7711);
#6346=AXIS2_PLACEMENT_3D('',#10263,#7712,#7713);
#6347=AXIS2_PLACEMENT_3D('',#10265,#7714,#7715);
#6348=AXIS2_PLACEMENT_3D('',#10267,#7716,#7717);
#6349=AXIS2_PLACEMENT_3D('',#10269,#7718,#7719);
#6350=AXIS2_PLACEMENT_3D('',#10271,#7720,#7721);
#6351=AXIS2_PLACEMENT_3D('',#10273,#7722,#7723);
#6352=AXIS2_PLACEMENT_3D('',#10275,#7724,#7725);
#6353=AXIS2_PLACEMENT_3D('',#10277,#7726,#7727);
#6354=AXIS2_PLACEMENT_3D('',#10279,#7728,#7729);
#6355=AXIS2_PLACEMENT_3D('',#10281,#7730,#7731);
#6356=AXIS2_PLACEMENT_3D('',#10283,#7732,#7733);
#6357=AXIS2_PLACEMENT_3D('',#10285,#7734,#7735);
#6358=AXIS2_PLACEMENT_3D('',#10287,#7736,#7737);
#6359=AXIS2_PLACEMENT_3D('',#10289,#7738,#7739);
#6360=AXIS2_PLACEMENT_3D('',#10291,#7740,#7741);
#6361=AXIS2_PLACEMENT_3D('',#10293,#7742,#7743);
#6362=AXIS2_PLACEMENT_3D('',#10295,#7744,#7745);
#6363=AXIS2_PLACEMENT_3D('',#10297,#7746,#7747);
#6364=AXIS2_PLACEMENT_3D('',#10299,#7748,#7749);
#6365=AXIS2_PLACEMENT_3D('',#10301,#7750,#7751);
#6366=AXIS2_PLACEMENT_3D('',#10303,#7752,#7753);
#6367=AXIS2_PLACEMENT_3D('',#10305,#7754,#7755);
#6368=AXIS2_PLACEMENT_3D('',#10307,#7756,#7757);
#6369=AXIS2_PLACEMENT_3D('',#10309,#7758,#7759);
#6370=AXIS2_PLACEMENT_3D('',#10311,#7760,#7761);
#6371=AXIS2_PLACEMENT_3D('',#10313,#7762,#7763);
#6372=AXIS2_PLACEMENT_3D('',#10315,#7764,#7765);
#6373=AXIS2_PLACEMENT_3D('',#10317,#7766,#7767);
#6374=AXIS2_PLACEMENT_3D('',#10319,#7768,#7769);
#6375=AXIS2_PLACEMENT_3D('',#10321,#7770,#7771);
#6376=AXIS2_PLACEMENT_3D('',#10323,#7772,#7773);
#6377=AXIS2_PLACEMENT_3D('',#10325,#7774,#7775);
#6378=AXIS2_PLACEMENT_3D('',#10327,#7776,#7777);
#6379=AXIS2_PLACEMENT_3D('',#10329,#7778,#7779);
#6380=AXIS2_PLACEMENT_3D('',#10331,#7780,#7781);
#6381=AXIS2_PLACEMENT_3D('',#10333,#7782,#7783);
#6382=AXIS2_PLACEMENT_3D('',#10335,#7784,#7785);
#6383=AXIS2_PLACEMENT_3D('',#10337,#7786,#7787);
#6384=AXIS2_PLACEMENT_3D('',#10339,#7788,#7789);
#6385=AXIS2_PLACEMENT_3D('',#10341,#7790,#7791);
#6386=AXIS2_PLACEMENT_3D('',#10343,#7792,#7793);
#6387=AXIS2_PLACEMENT_3D('',#10345,#7794,#7795);
#6388=AXIS2_PLACEMENT_3D('',#10347,#7796,#7797);
#6389=AXIS2_PLACEMENT_3D('',#10349,#7798,#7799);
#6390=AXIS2_PLACEMENT_3D('',#10351,#7800,#7801);
#6391=AXIS2_PLACEMENT_3D('',#10352,#7802,#7803);
#6392=AXIS2_PLACEMENT_3D('',#10353,#7804,#7805);
#6393=AXIS2_PLACEMENT_3D('',#10355,#7807,#7808);
#6394=AXIS2_PLACEMENT_3D('',#10358,#7811,#7812);
#6395=AXIS2_PLACEMENT_3D('',#10360,#7814,#7815);
#6396=AXIS2_PLACEMENT_3D('',#10362,#7817,#7818);
#6397=AXIS2_PLACEMENT_3D('',#10364,#7820,#7821);
#6398=AXIS2_PLACEMENT_3D('',#10366,#7823,#7824);
#6399=AXIS2_PLACEMENT_3D('',#10368,#7826,#7827);
#6400=AXIS2_PLACEMENT_3D('',#10370,#7829,#7830);
#6401=AXIS2_PLACEMENT_3D('',#10372,#7832,#7833);
#6402=AXIS2_PLACEMENT_3D('',#10374,#7835,#7836);
#6403=AXIS2_PLACEMENT_3D('',#10376,#7838,#7839);
#6404=AXIS2_PLACEMENT_3D('',#10378,#7841,#7842);
#6405=AXIS2_PLACEMENT_3D('',#10380,#7844,#7845);
#6406=AXIS2_PLACEMENT_3D('',#10382,#7847,#7848);
#6407=AXIS2_PLACEMENT_3D('',#10384,#7850,#7851);
#6408=AXIS2_PLACEMENT_3D('',#10386,#7853,#7854);
#6409=AXIS2_PLACEMENT_3D('',#10388,#7856,#7857);
#6410=AXIS2_PLACEMENT_3D('',#10390,#7859,#7860);
#6411=AXIS2_PLACEMENT_3D('',#10392,#7862,#7863);
#6412=AXIS2_PLACEMENT_3D('',#10394,#7865,#7866);
#6413=AXIS2_PLACEMENT_3D('',#10396,#7868,#7869);
#6414=AXIS2_PLACEMENT_3D('',#10398,#7871,#7872);
#6415=AXIS2_PLACEMENT_3D('',#10400,#7874,#7875);
#6416=AXIS2_PLACEMENT_3D('',#10402,#7877,#7878);
#6417=AXIS2_PLACEMENT_3D('',#10404,#7880,#7881);
#6418=AXIS2_PLACEMENT_3D('',#10406,#7883,#7884);
#6419=AXIS2_PLACEMENT_3D('',#10408,#7886,#7887);
#6420=AXIS2_PLACEMENT_3D('',#10410,#7889,#7890);
#6421=AXIS2_PLACEMENT_3D('',#10412,#7892,#7893);
#6422=AXIS2_PLACEMENT_3D('',#10414,#7895,#7896);
#6423=AXIS2_PLACEMENT_3D('',#10416,#7898,#7899);
#6424=AXIS2_PLACEMENT_3D('',#10418,#7901,#7902);
#6425=AXIS2_PLACEMENT_3D('',#10420,#7904,#7905);
#6426=AXIS2_PLACEMENT_3D('',#10422,#7907,#7908);
#6427=AXIS2_PLACEMENT_3D('',#10424,#7910,#7911);
#6428=AXIS2_PLACEMENT_3D('',#10426,#7913,#7914);
#6429=AXIS2_PLACEMENT_3D('',#10428,#7916,#7917);
#6430=AXIS2_PLACEMENT_3D('',#10430,#7919,#7920);
#6431=AXIS2_PLACEMENT_3D('',#10432,#7922,#7923);
#6432=AXIS2_PLACEMENT_3D('',#10434,#7925,#7926);
#6433=AXIS2_PLACEMENT_3D('',#10436,#7928,#7929);
#6434=AXIS2_PLACEMENT_3D('',#10438,#7931,#7932);
#6435=AXIS2_PLACEMENT_3D('',#10440,#7934,#7935);
#6436=AXIS2_PLACEMENT_3D('',#10442,#7937,#7938);
#6437=AXIS2_PLACEMENT_3D('',#10444,#7940,#7941);
#6438=AXIS2_PLACEMENT_3D('',#10446,#7943,#7944);
#6439=AXIS2_PLACEMENT_3D('',#10448,#7946,#7947);
#6440=AXIS2_PLACEMENT_3D('',#10450,#7949,#7950);
#6441=AXIS2_PLACEMENT_3D('',#10452,#7952,#7953);
#6442=AXIS2_PLACEMENT_3D('',#10454,#7955,#7956);
#6443=AXIS2_PLACEMENT_3D('',#10456,#7958,#7959);
#6444=AXIS2_PLACEMENT_3D('',#10458,#7961,#7962);
#6445=AXIS2_PLACEMENT_3D('',#10460,#7964,#7965);
#6446=AXIS2_PLACEMENT_3D('',#10462,#7967,#7968);
#6447=AXIS2_PLACEMENT_3D('',#10464,#7970,#7971);
#6448=AXIS2_PLACEMENT_3D('',#10466,#7973,#7974);
#6449=AXIS2_PLACEMENT_3D('',#10468,#7976,#7977);
#6450=AXIS2_PLACEMENT_3D('',#10470,#7979,#7980);
#6451=AXIS2_PLACEMENT_3D('',#10472,#7982,#7983);
#6452=AXIS2_PLACEMENT_3D('',#10474,#7985,#7986);
#6453=AXIS2_PLACEMENT_3D('',#10476,#7988,#7989);
#6454=AXIS2_PLACEMENT_3D('',#10478,#7991,#7992);
#6455=AXIS2_PLACEMENT_3D('',#10480,#7994,#7995);
#6456=AXIS2_PLACEMENT_3D('',#10482,#7997,#7998);
#6457=AXIS2_PLACEMENT_3D('',#10484,#8000,#8001);
#6458=AXIS2_PLACEMENT_3D('',#10486,#8003,#8004);
#6459=AXIS2_PLACEMENT_3D('',#10488,#8006,#8007);
#6460=AXIS2_PLACEMENT_3D('',#10490,#8009,#8010);
#6461=AXIS2_PLACEMENT_3D('',#10492,#8012,#8013);
#6462=AXIS2_PLACEMENT_3D('',#10494,#8015,#8016);
#6463=AXIS2_PLACEMENT_3D('',#10496,#8018,#8019);
#6464=AXIS2_PLACEMENT_3D('',#10498,#8021,#8022);
#6465=AXIS2_PLACEMENT_3D('',#10500,#8024,#8025);
#6466=AXIS2_PLACEMENT_3D('',#10502,#8027,#8028);
#6467=AXIS2_PLACEMENT_3D('',#10504,#8030,#8031);
#6468=AXIS2_PLACEMENT_3D('',#10506,#8033,#8034);
#6469=AXIS2_PLACEMENT_3D('',#10508,#8036,#8037);
#6470=AXIS2_PLACEMENT_3D('',#10510,#8039,#8040);
#6471=AXIS2_PLACEMENT_3D('',#10512,#8042,#8043);
#6472=AXIS2_PLACEMENT_3D('',#10514,#8045,#8046);
#6473=AXIS2_PLACEMENT_3D('',#10515,#8047,#8048);
#6474=AXIS2_PLACEMENT_3D('',#10516,#8049,#8050);
#6475=AXIS2_PLACEMENT_3D('',#10533,#8059,#8060);
#6476=AXIS2_PLACEMENT_3D('',#10539,#8064,#8065);
#6477=AXIS2_PLACEMENT_3D('',#10543,#8068,#8069);
#6478=AXIS2_PLACEMENT_3D('',#10547,#8072,#8073);
#6479=AXIS2_PLACEMENT_3D('',#10551,#8076,#8077);
#6480=AXIS2_PLACEMENT_3D('',#10559,#8082,#8083);
#6481=AXIS2_PLACEMENT_3D('',#10561,#8085,#8086);
#6482=AXIS2_PLACEMENT_3D('',#10563,#8088,#8089);
#6483=AXIS2_PLACEMENT_3D('',#10565,#8091,#8092);
#6484=AXIS2_PLACEMENT_3D('',#10566,#8093,#8094);
#6485=AXIS2_PLACEMENT_3D('',#10567,#8095,#8096);
#6486=AXIS2_PLACEMENT_3D('',#10569,#8097,#8098);
#6487=AXIS2_PLACEMENT_3D('',#10570,#8099,#8100);
#6488=AXIS2_PLACEMENT_3D('',#10572,#8101,#8102);
#6489=AXIS2_PLACEMENT_3D('',#10574,#8104,#8105);
#6490=AXIS2_PLACEMENT_3D('',#10576,#8106,#8107);
#6491=AXIS2_PLACEMENT_3D('',#10578,#8109,#8110);
#6492=AXIS2_PLACEMENT_3D('',#10580,#8111,#8112);
#6493=AXIS2_PLACEMENT_3D('',#10582,#8114,#8115);
#6494=AXIS2_PLACEMENT_3D('',#10584,#8116,#8117);
#6495=AXIS2_PLACEMENT_3D('',#10585,#8118,#8119);
#6496=AXIS2_PLACEMENT_3D('',#10587,#8120,#8121);
#6497=AXIS2_PLACEMENT_3D('',#10589,#8123,#8124);
#6498=AXIS2_PLACEMENT_3D('',#10591,#8125,#8126);
#6499=AXIS2_PLACEMENT_3D('',#10593,#8128,#8129);
#6500=AXIS2_PLACEMENT_3D('',#10595,#8130,#8131);
#6501=AXIS2_PLACEMENT_3D('',#10597,#8133,#8134);
#6502=AXIS2_PLACEMENT_3D('',#10598,#8135,#8136);
#6503=AXIS2_PLACEMENT_3D('',#10607,#8141,#8142);
#6504=AXIS2_PLACEMENT_3D('',#10613,#8146,#8147);
#6505=AXIS2_PLACEMENT_3D('',#10619,#8151,#8152);
#6506=AXIS2_PLACEMENT_3D('',#10625,#8156,#8157);
#6507=AXIS2_PLACEMENT_3D('',#10631,#8161,#8162);
#6508=AXIS2_PLACEMENT_3D('',#10634,#8165,#8166);
#6509=AXIS2_PLACEMENT_3D('',#10635,#8167,#8168);
#6510=AXIS2_PLACEMENT_3D('',#10636,#8169,#8170);
#6511=AXIS2_PLACEMENT_3D('',#10637,#8171,#8172);
#6512=AXIS2_PLACEMENT_3D('',#10654,#8181,#8182);
#6513=AXIS2_PLACEMENT_3D('',#10660,#8186,#8187);
#6514=AXIS2_PLACEMENT_3D('',#10664,#8190,#8191);
#6515=AXIS2_PLACEMENT_3D('',#10668,#8194,#8195);
#6516=AXIS2_PLACEMENT_3D('',#10672,#8198,#8199);
#6517=AXIS2_PLACEMENT_3D('',#10680,#8204,#8205);
#6518=AXIS2_PLACEMENT_3D('',#10682,#8207,#8208);
#6519=AXIS2_PLACEMENT_3D('',#10684,#8210,#8211);
#6520=AXIS2_PLACEMENT_3D('',#10686,#8213,#8214);
#6521=AXIS2_PLACEMENT_3D('',#10687,#8215,#8216);
#6522=AXIS2_PLACEMENT_3D('',#10688,#8217,#8218);
#6523=AXIS2_PLACEMENT_3D('',#10697,#8223,#8224);
#6524=AXIS2_PLACEMENT_3D('',#10703,#8228,#8229);
#6525=AXIS2_PLACEMENT_3D('',#10709,#8233,#8234);
#6526=AXIS2_PLACEMENT_3D('',#10715,#8238,#8239);
#6527=AXIS2_PLACEMENT_3D('',#10721,#8243,#8244);
#6528=AXIS2_PLACEMENT_3D('',#10724,#8247,#8248);
#6529=AXIS2_PLACEMENT_3D('',#10725,#8249,#8250);
#6530=AXIS2_PLACEMENT_3D('',#10727,#8251,#8252);
#6531=AXIS2_PLACEMENT_3D('',#10728,#8253,#8254);
#6532=AXIS2_PLACEMENT_3D('',#10730,#8255,#8256);
#6533=AXIS2_PLACEMENT_3D('',#10732,#8258,#8259);
#6534=AXIS2_PLACEMENT_3D('',#10734,#8260,#8261);
#6535=AXIS2_PLACEMENT_3D('',#10736,#8263,#8264);
#6536=AXIS2_PLACEMENT_3D('',#10738,#8265,#8266);
#6537=AXIS2_PLACEMENT_3D('',#10740,#8268,#8269);
#6538=AXIS2_PLACEMENT_3D('',#10741,#8270,#8271);
#6539=AXIS2_PLACEMENT_3D('',#10742,#8272,#8273);
#6540=AXIS2_PLACEMENT_3D('',#10743,#8274,#8275);
#6541=AXIS2_PLACEMENT_3D('',#10744,#8276,#8277);
#6542=AXIS2_PLACEMENT_3D('',#10745,#8278,#8279);
#6543=AXIS2_PLACEMENT_3D('',#10746,#8280,#8281);
#6544=AXIS2_PLACEMENT_3D('',#10747,#8282,#8283);
#6545=AXIS2_PLACEMENT_3D('',#10748,#8284,#8285);
#6546=AXIS2_PLACEMENT_3D('',#10749,#8286,#8287);
#6547=AXIS2_PLACEMENT_3D('',#10750,#8288,#8289);
#6548=AXIS2_PLACEMENT_3D('',#10751,#8290,#8291);
#6549=AXIS2_PLACEMENT_3D('',#10752,#8292,#8293);
#6550=AXIS2_PLACEMENT_3D('',#10753,#8294,#8295);
#6551=AXIS2_PLACEMENT_3D('',#10754,#8296,#8297);
#6552=AXIS2_PLACEMENT_3D('',#10755,#8298,#8299);
#6553=AXIS2_PLACEMENT_3D('',#10756,#8300,#8301);
#6554=AXIS2_PLACEMENT_3D('',#10757,#8302,#8303);
#6555=AXIS2_PLACEMENT_3D('',#10758,#8304,#8305);
#6556=AXIS2_PLACEMENT_3D('',#10759,#8306,#8307);
#6557=AXIS2_PLACEMENT_3D('',#10760,#8308,#8309);
#6558=AXIS2_PLACEMENT_3D('',#10761,#8310,#8311);
#6559=DIRECTION('axis',(0.,0.,1.));
#6560=DIRECTION('refdir',(1.,0.,0.));
#6561=DIRECTION('axis',(0.,0.,1.));
#6562=DIRECTION('refdir',(1.,0.,0.));
#6563=DIRECTION('axis',(0.,0.,1.));
#6564=DIRECTION('refdir',(1.,0.,0.));
#6565=DIRECTION('center_axis',(0.,0.,1.));
#6566=DIRECTION('ref_axis',(1.,0.,0.));
#6567=DIRECTION('center_axis',(0.,0.,1.));
#6568=DIRECTION('ref_axis',(1.,0.,0.));
#6569=DIRECTION('',(0.,0.,1.));
#6570=DIRECTION('center_axis',(0.,0.,-1.));
#6571=DIRECTION('ref_axis',(1.,0.,0.));
#6572=DIRECTION('center_axis',(0.,0.,1.));
#6573=DIRECTION('ref_axis',(1.,0.,0.));
#6574=DIRECTION('center_axis',(0.,0.,1.));
#6575=DIRECTION('ref_axis',(1.,0.,0.));
#6576=DIRECTION('',(0.,0.,1.));
#6577=DIRECTION('center_axis',(0.,0.,-1.));
#6578=DIRECTION('ref_axis',(1.,0.,0.));
#6579=DIRECTION('center_axis',(0.,0.,1.));
#6580=DIRECTION('ref_axis',(1.,0.,0.));
#6581=DIRECTION('center_axis',(0.,0.,1.));
#6582=DIRECTION('ref_axis',(1.,0.,0.));
#6583=DIRECTION('',(0.,0.,1.));
#6584=DIRECTION('center_axis',(0.,0.,-1.));
#6585=DIRECTION('ref_axis',(1.,0.,0.));
#6586=DIRECTION('center_axis',(0.,0.,1.));
#6587=DIRECTION('ref_axis',(1.,0.,0.));
#6588=DIRECTION('center_axis',(0.,0.,1.));
#6589=DIRECTION('ref_axis',(1.,0.,0.));
#6590=DIRECTION('',(0.,0.,1.));
#6591=DIRECTION('center_axis',(0.,0.,-1.));
#6592=DIRECTION('ref_axis',(1.,0.,0.));
#6593=DIRECTION('center_axis',(0.,1.,0.));
#6594=DIRECTION('ref_axis',(-1.,0.,0.));
#6595=DIRECTION('',(-1.,0.,0.));
#6596=DIRECTION('',(0.,0.,1.));
#6597=DIRECTION('',(-1.,0.,0.));
#6598=DIRECTION('',(0.,0.,1.));
#6599=DIRECTION('center_axis',(1.,0.,0.));
#6600=DIRECTION('ref_axis',(0.,1.,0.));
#6601=DIRECTION('',(0.,1.,0.));
#6602=DIRECTION('',(0.,1.,0.));
#6603=DIRECTION('',(0.,0.,1.));
#6604=DIRECTION('center_axis',(0.,-1.,0.));
#6605=DIRECTION('ref_axis',(1.,0.,0.));
#6606=DIRECTION('',(1.,0.,0.));
#6607=DIRECTION('',(1.,0.,0.));
#6608=DIRECTION('',(0.,0.,1.));
#6609=DIRECTION('center_axis',(-1.,0.,0.));
#6610=DIRECTION('ref_axis',(0.,-1.,0.));
#6611=DIRECTION('',(0.,-1.,0.));
#6612=DIRECTION('',(0.,-1.,0.));
#6613=DIRECTION('center_axis',(0.,0.,1.));
#6614=DIRECTION('ref_axis',(1.,0.,0.));
#6615=DIRECTION('center_axis',(0.,0.,1.));
#6616=DIRECTION('ref_axis',(1.,0.,0.));
#6617=DIRECTION('axis',(0.,0.,1.));
#6618=DIRECTION('refdir',(1.,0.,0.));
#6619=DIRECTION('center_axis',(0.,1.,0.));
#6620=DIRECTION('ref_axis',(-1.,0.,0.));
#6621=DIRECTION('',(-1.,0.,0.));
#6622=DIRECTION('',(0.,0.,1.));
#6623=DIRECTION('',(-1.,0.,0.));
#6624=DIRECTION('',(0.,0.,1.));
#6625=DIRECTION('center_axis',(1.,0.,0.));
#6626=DIRECTION('ref_axis',(0.,1.,0.));
#6627=DIRECTION('',(0.,1.,0.));
#6628=DIRECTION('',(0.,1.,0.));
#6629=DIRECTION('',(0.,0.,1.));
#6630=DIRECTION('center_axis',(0.,-1.,0.));
#6631=DIRECTION('ref_axis',(1.,0.,0.));
#6632=DIRECTION('',(1.,0.,0.));
#6633=DIRECTION('',(1.,0.,0.));
#6634=DIRECTION('',(0.,0.,1.));
#6635=DIRECTION('center_axis',(-1.,0.,0.));
#6636=DIRECTION('ref_axis',(0.,-1.,0.));
#6637=DIRECTION('',(0.,-1.,0.));
#6638=DIRECTION('',(0.,-1.,0.));
#6639=DIRECTION('center_axis',(0.,0.,1.));
#6640=DIRECTION('ref_axis',(1.,0.,0.));
#6641=DIRECTION('center_axis',(0.,0.,1.));
#6642=DIRECTION('ref_axis',(1.,0.,0.));
#6643=DIRECTION('axis',(0.,0.,1.));
#6644=DIRECTION('refdir',(1.,0.,0.));
#6645=DIRECTION('center_axis',(0.,1.,0.));
#6646=DIRECTION('ref_axis',(-1.,0.,0.));
#6647=DIRECTION('',(-1.,0.,0.));
#6648=DIRECTION('',(0.,0.,1.));
#6649=DIRECTION('',(-1.,0.,0.));
#6650=DIRECTION('',(0.,0.,1.));
#6651=DIRECTION('center_axis',(1.,0.,0.));
#6652=DIRECTION('ref_axis',(0.,1.,0.));
#6653=DIRECTION('',(0.,1.,0.));
#6654=DIRECTION('',(0.,1.,0.));
#6655=DIRECTION('',(0.,0.,1.));
#6656=DIRECTION('center_axis',(0.,-1.,0.));
#6657=DIRECTION('ref_axis',(1.,0.,0.));
#6658=DIRECTION('',(1.,0.,0.));
#6659=DIRECTION('',(1.,0.,0.));
#6660=DIRECTION('',(0.,0.,1.));
#6661=DIRECTION('center_axis',(-1.,0.,0.));
#6662=DIRECTION('ref_axis',(0.,-1.,0.));
#6663=DIRECTION('',(0.,-1.,0.));
#6664=DIRECTION('',(0.,-1.,0.));
#6665=DIRECTION('center_axis',(0.,0.,1.));
#6666=DIRECTION('ref_axis',(1.,0.,0.));
#6667=DIRECTION('center_axis',(0.,0.,1.));
#6668=DIRECTION('ref_axis',(1.,0.,0.));
#6669=DIRECTION('axis',(0.,0.,1.));
#6670=DIRECTION('refdir',(1.,0.,0.));
#6671=DIRECTION('center_axis',(0.,0.,1.));
#6672=DIRECTION('ref_axis',(1.,0.,0.));
#6673=DIRECTION('center_axis',(0.,0.,-1.));
#6674=DIRECTION('ref_axis',(1.,0.,0.));
#6675=DIRECTION('',(0.,0.,-1.));
#6676=DIRECTION('center_axis',(0.,0.,-1.));
#6677=DIRECTION('ref_axis',(1.,0.,0.));
#6678=DIRECTION('center_axis',(0.,0.,1.));
#6679=DIRECTION('ref_axis',(1.,0.,0.));
#6680=DIRECTION('center_axis',(0.,0.,1.));
#6681=DIRECTION('ref_axis',(1.,0.,0.));
#6682=DIRECTION('',(0.,0.,-1.));
#6683=DIRECTION('center_axis',(0.,0.,1.));
#6684=DIRECTION('ref_axis',(1.,0.,0.));
#6685=DIRECTION('center_axis',(0.,0.,1.));
#6686=DIRECTION('ref_axis',(1.,0.,0.));
#6687=DIRECTION('center_axis',(0.,0.,1.));
#6688=DIRECTION('ref_axis',(1.,0.,0.));
#6689=DIRECTION('axis',(0.,0.,1.));
#6690=DIRECTION('refdir',(1.,0.,0.));
#6691=DIRECTION('center_axis',(0.,0.,1.));
#6692=DIRECTION('ref_axis',(1.,0.,0.));
#6693=DIRECTION('center_axis',(0.,0.,-1.));
#6694=DIRECTION('ref_axis',(1.,0.,0.));
#6695=DIRECTION('',(0.,0.,-1.));
#6696=DIRECTION('center_axis',(0.,0.,-1.));
#6697=DIRECTION('ref_axis',(1.,0.,0.));
#6698=DIRECTION('center_axis',(0.,0.,1.));
#6699=DIRECTION('ref_axis',(1.,0.,0.));
#6700=DIRECTION('center_axis',(0.,0.,1.));
#6701=DIRECTION('ref_axis',(1.,0.,0.));
#6702=DIRECTION('',(0.,0.,-1.));
#6703=DIRECTION('center_axis',(0.,0.,1.));
#6704=DIRECTION('ref_axis',(1.,0.,0.));
#6705=DIRECTION('center_axis',(0.,0.,1.));
#6706=DIRECTION('ref_axis',(1.,0.,0.));
#6707=DIRECTION('center_axis',(0.,0.,1.));
#6708=DIRECTION('ref_axis',(1.,0.,0.));
#6709=DIRECTION('axis',(0.,0.,1.));
#6710=DIRECTION('refdir',(1.,0.,0.));
#6711=DIRECTION('center_axis',(0.,0.,1.));
#6712=DIRECTION('ref_axis',(1.,0.,0.));
#6713=DIRECTION('center_axis',(0.,0.,-1.));
#6714=DIRECTION('ref_axis',(1.,0.,0.));
#6715=DIRECTION('',(0.,0.,-1.));
#6716=DIRECTION('center_axis',(0.,0.,-1.));
#6717=DIRECTION('ref_axis',(1.,0.,0.));
#6718=DIRECTION('center_axis',(0.,0.,1.));
#6719=DIRECTION('ref_axis',(1.,0.,0.));
#6720=DIRECTION('center_axis',(0.,0.,1.));
#6721=DIRECTION('ref_axis',(1.,0.,0.));
#6722=DIRECTION('',(0.,0.,-1.));
#6723=DIRECTION('center_axis',(0.,0.,1.));
#6724=DIRECTION('ref_axis',(1.,0.,0.));
#6725=DIRECTION('center_axis',(0.,0.,1.));
#6726=DIRECTION('ref_axis',(1.,0.,0.));
#6727=DIRECTION('center_axis',(0.,0.,1.));
#6728=DIRECTION('ref_axis',(1.,0.,0.));
#6729=DIRECTION('axis',(0.,0.,1.));
#6730=DIRECTION('refdir',(1.,0.,0.));
#6731=DIRECTION('center_axis',(0.,0.,1.));
#6732=DIRECTION('ref_axis',(1.,0.,0.));
#6733=DIRECTION('center_axis',(0.,0.,-1.));
#6734=DIRECTION('ref_axis',(1.,0.,0.));
#6735=DIRECTION('',(0.,0.,-1.));
#6736=DIRECTION('center_axis',(0.,0.,-1.));
#6737=DIRECTION('ref_axis',(1.,0.,0.));
#6738=DIRECTION('center_axis',(0.,0.,1.));
#6739=DIRECTION('ref_axis',(1.,0.,0.));
#6740=DIRECTION('center_axis',(0.,0.,1.));
#6741=DIRECTION('ref_axis',(1.,0.,0.));
#6742=DIRECTION('',(0.,0.,-1.));
#6743=DIRECTION('center_axis',(0.,0.,1.));
#6744=DIRECTION('ref_axis',(1.,0.,0.));
#6745=DIRECTION('center_axis',(0.,0.,1.));
#6746=DIRECTION('ref_axis',(1.,0.,0.));
#6747=DIRECTION('center_axis',(0.,0.,1.));
#6748=DIRECTION('ref_axis',(1.,0.,0.));
#6749=DIRECTION('axis',(0.,0.,1.));
#6750=DIRECTION('refdir',(1.,0.,0.));
#6751=DIRECTION('axis',(0.,0.,1.));
#6752=DIRECTION('refdir',(1.,0.,0.));
#6753=DIRECTION('center_axis',(0.,1.,0.));
#6754=DIRECTION('ref_axis',(1.,0.,0.));
#6755=DIRECTION('center_axis',(0.,1.,0.));
#6756=DIRECTION('ref_axis',(1.,0.,0.));
#6757=DIRECTION('',(0.,1.,0.));
#6758=DIRECTION('center_axis',(0.,-1.,0.));
#6759=DIRECTION('ref_axis',(1.,0.,0.));
#6760=DIRECTION('center_axis',(0.,1.,0.));
#6761=DIRECTION('ref_axis',(1.,0.,0.));
#6762=DIRECTION('center_axis',(0.,1.,0.));
#6763=DIRECTION('ref_axis',(1.,0.,0.));
#6764=DIRECTION('',(0.,1.,0.));
#6765=DIRECTION('center_axis',(0.,-1.,0.));
#6766=DIRECTION('ref_axis',(1.,0.,0.));
#6767=DIRECTION('center_axis',(6.12323399573677E-17,0.,1.));
#6768=DIRECTION('ref_axis',(1.,0.,0.));
#6769=DIRECTION('center_axis',(-1.22464679914735E-16,1.,0.));
#6770=DIRECTION('ref_axis',(-1.,-1.22464679914735E-16,0.));
#6771=DIRECTION('center_axis',(0.,1.,0.));
#6772=DIRECTION('ref_axis',(0.,0.,1.));
#6773=DIRECTION('',(1.,0.,0.));
#6774=DIRECTION('',(0.850265146687862,0.,0.526354614616295));
#6775=DIRECTION('center_axis',(0.,1.,0.));
#6776=DIRECTION('ref_axis',(1.,0.,0.));
#6777=DIRECTION('center_axis',(0.,1.,0.));
#6778=DIRECTION('ref_axis',(0.,0.,1.));
#6779=DIRECTION('',(1.,0.,0.));
#6780=DIRECTION('center_axis',(0.,1.,0.));
#6781=DIRECTION('ref_axis',(1.,0.,0.));
#6782=DIRECTION('',(0.850265146687862,0.,-0.526354614616295));
#6783=DIRECTION('center_axis',(0.,-1.,0.));
#6784=DIRECTION('ref_axis',(0.,0.,-1.));
#6785=DIRECTION('',(-1.,0.,0.));
#6786=DIRECTION('center_axis',(0.,-1.,0.));
#6787=DIRECTION('ref_axis',(1.,0.,0.));
#6788=DIRECTION('',(-0.850265146687862,0.,-0.526354614616295));
#6789=DIRECTION('center_axis',(-0.526354614616295,0.,0.850265146687862));
#6790=DIRECTION('ref_axis',(0.850265146687862,0.,0.526354614616295));
#6791=DIRECTION('',(0.,1.,0.));
#6792=DIRECTION('',(0.,-1.,0.));
#6793=DIRECTION('center_axis',(0.,-1.,0.));
#6794=DIRECTION('ref_axis',(0.,0.,-1.));
#6795=DIRECTION('',(-1.,0.,0.));
#6796=DIRECTION('',(-0.850265146687862,0.,0.526354614616295));
#6797=DIRECTION('center_axis',(0.,-1.,0.));
#6798=DIRECTION('ref_axis',(1.,0.,0.));
#6799=DIRECTION('center_axis',(0.526354614616295,0.,0.850265146687862));
#6800=DIRECTION('ref_axis',(0.850265146687862,0.,-0.526354614616295));
#6801=DIRECTION('',(0.,-1.,0.));
#6802=DIRECTION('',(0.,1.,0.));
#6803=DIRECTION('center_axis',(0.,0.,1.));
#6804=DIRECTION('ref_axis',(1.,0.,0.));
#6805=DIRECTION('',(0.,-1.,0.));
#6806=DIRECTION('',(1.,0.,0.));
#6807=DIRECTION('',(0.,1.,0.));
#6808=DIRECTION('',(-1.,0.,0.));
#6809=DIRECTION('center_axis',(0.,0.,-1.));
#6810=DIRECTION('ref_axis',(1.,0.,0.));
#6811=DIRECTION('center_axis',(0.,0.,-1.));
#6812=DIRECTION('ref_axis',(1.,0.,0.));
#6813=DIRECTION('',(0.,-1.,0.));
#6814=DIRECTION('',(-1.,0.,0.));
#6815=DIRECTION('',(0.,1.,0.));
#6816=DIRECTION('',(0.,1.,0.));
#6817=DIRECTION('',(1.,0.,0.));
#6818=DIRECTION('',(0.,-1.,0.));
#6819=DIRECTION('center_axis',(0.,1.,0.));
#6820=DIRECTION('ref_axis',(6.12323399573677E-17,0.,1.));
#6821=DIRECTION('center_axis',(0.,1.,0.));
#6822=DIRECTION('ref_axis',(1.,0.,0.));
#6823=DIRECTION('center_axis',(0.,-1.,0.));
#6824=DIRECTION('ref_axis',(1.,0.,0.));
#6825=DIRECTION('center_axis',(0.,1.,0.));
#6826=DIRECTION('ref_axis',(1.,0.,0.));
#6827=DIRECTION('center_axis',(0.,1.,0.));
#6828=DIRECTION('ref_axis',(1.,0.,0.));
#6829=DIRECTION('center_axis',(0.,1.,0.));
#6830=DIRECTION('ref_axis',(-1.,0.,0.));
#6831=DIRECTION('',(-1.,0.,0.));
#6832=DIRECTION('',(0.,0.,1.));
#6833=DIRECTION('',(-1.,0.,0.));
#6834=DIRECTION('',(0.,0.,1.));
#6835=DIRECTION('center_axis',(1.,0.,0.));
#6836=DIRECTION('ref_axis',(0.,1.,0.));
#6837=DIRECTION('',(0.,1.,0.));
#6838=DIRECTION('',(0.,0.,1.));
#6839=DIRECTION('',(0.,1.,0.));
#6840=DIRECTION('center_axis',(0.,-1.,0.));
#6841=DIRECTION('ref_axis',(1.,0.,0.));
#6842=DIRECTION('',(1.,0.,0.));
#6843=DIRECTION('',(0.,0.,1.));
#6844=DIRECTION('',(1.,0.,0.));
#6845=DIRECTION('center_axis',(-1.,0.,0.));
#6846=DIRECTION('ref_axis',(0.,-1.,0.));
#6847=DIRECTION('',(0.,-1.,0.));
#6848=DIRECTION('',(0.,-1.,0.));
#6849=DIRECTION('center_axis',(0.,0.,1.));
#6850=DIRECTION('ref_axis',(1.,0.,0.));
#6851=DIRECTION('center_axis',(0.,0.,1.));
#6852=DIRECTION('ref_axis',(1.,0.,0.));
#6853=DIRECTION('center_axis',(0.,0.,1.));
#6854=DIRECTION('ref_axis',(1.,0.,0.));
#6855=DIRECTION('',(0.,0.,1.));
#6856=DIRECTION('center_axis',(0.,0.,1.));
#6857=DIRECTION('ref_axis',(1.,0.,0.));
#6858=DIRECTION('center_axis',(0.,0.,1.));
#6859=DIRECTION('ref_axis',(1.,0.,0.));
#6860=DIRECTION('',(0.,0.,1.));
#6861=DIRECTION('center_axis',(0.,1.,0.));
#6862=DIRECTION('ref_axis',(-1.,0.,0.));
#6863=DIRECTION('',(-1.,0.,0.));
#6864=DIRECTION('',(0.,0.,1.));
#6865=DIRECTION('',(0.,0.,1.));
#6866=DIRECTION('center_axis',(1.,0.,0.));
#6867=DIRECTION('ref_axis',(0.,1.,0.));
#6868=DIRECTION('',(0.,1.,0.));
#6869=DIRECTION('',(0.,0.,1.));
#6870=DIRECTION('center_axis',(0.,-1.,0.));
#6871=DIRECTION('ref_axis',(1.,0.,0.));
#6872=DIRECTION('',(1.,0.,0.));
#6873=DIRECTION('',(0.,0.,1.));
#6874=DIRECTION('center_axis',(-1.,0.,0.));
#6875=DIRECTION('ref_axis',(0.,-1.,0.));
#6876=DIRECTION('',(0.,-1.,0.));
#6877=DIRECTION('center_axis',(0.,0.,1.));
#6878=DIRECTION('ref_axis',(1.,0.,0.));
#6879=DIRECTION('axis',(0.,0.,1.));
#6880=DIRECTION('refdir',(1.,0.,0.));
#6881=DIRECTION('center_axis',(0.,-1.,0.));
#6882=DIRECTION('ref_axis',(1.,0.,0.));
#6883=DIRECTION('center_axis',(0.,-1.,0.));
#6884=DIRECTION('ref_axis',(1.,0.,0.));
#6885=DIRECTION('',(0.,1.,0.));
#6886=DIRECTION('center_axis',(0.,-1.,0.));
#6887=DIRECTION('ref_axis',(1.,0.,0.));
#6888=DIRECTION('center_axis',(0.,1.,0.));
#6889=DIRECTION('ref_axis',(0.,0.,1.));
#6890=DIRECTION('center_axis',(0.,-1.,0.));
#6891=DIRECTION('ref_axis',(1.,0.,0.));
#6892=DIRECTION('center_axis',(6.12323399573677E-17,0.,1.));
#6893=DIRECTION('ref_axis',(1.,0.,0.));
#6894=DIRECTION('center_axis',(1.22464679914735E-16,-1.,0.));
#6895=DIRECTION('ref_axis',(-1.,-1.22464679914735E-16,0.));
#6896=DIRECTION('center_axis',(0.,-1.,0.));
#6897=DIRECTION('ref_axis',(1.,0.,0.));
#6898=DIRECTION('center_axis',(0.,-1.,0.));
#6899=DIRECTION('ref_axis',(0.,0.,-1.));
#6900=DIRECTION('center_axis',(-0.866025403784438,0.,-0.5));
#6901=DIRECTION('ref_axis',(-0.5,0.,0.866025403784438));
#6902=DIRECTION('',(-0.866025403784438,0.,-0.5));
#6903=DIRECTION('center_axis',(-0.866025403784438,0.,-0.5));
#6904=DIRECTION('ref_axis',(-0.5,0.,0.866025403784438));
#6905=DIRECTION('',(-0.866025403784438,0.,-0.5));
#6906=DIRECTION('center_axis',(0.,-1.,0.));
#6907=DIRECTION('ref_axis',(1.,0.,0.));
#6908=DIRECTION('center_axis',(0.,-1.,0.));
#6909=DIRECTION('ref_axis',(1.,0.,0.));
#6910=DIRECTION('',(0.,1.,0.));
#6911=DIRECTION('center_axis',(0.,-1.,0.));
#6912=DIRECTION('ref_axis',(1.,0.,0.));
#6913=DIRECTION('center_axis',(0.866025403784439,0.,-0.5));
#6914=DIRECTION('ref_axis',(-0.5,0.,-0.866025403784439));
#6915=DIRECTION('',(0.866025403784439,0.,-0.5));
#6916=DIRECTION('center_axis',(0.866025403784439,0.,-0.5));
#6917=DIRECTION('ref_axis',(-0.5,0.,-0.866025403784439));
#6918=DIRECTION('',(0.866025403784439,0.,-0.5));
#6919=DIRECTION('center_axis',(0.,0.,1.));
#6920=DIRECTION('ref_axis',(1.,0.,0.));
#6921=DIRECTION('',(0.,0.,1.));
#6922=DIRECTION('center_axis',(0.,0.,1.));
#6923=DIRECTION('ref_axis',(1.,0.,0.));
#6924=DIRECTION('',(0.,0.,1.));
#6925=DIRECTION('center_axis',(0.,1.,0.));
#6926=DIRECTION('ref_axis',(0.,0.,1.));
#6927=DIRECTION('center_axis',(0.,-1.,0.));
#6928=DIRECTION('ref_axis',(1.,0.,0.));
#6929=DIRECTION('center_axis',(0.,1.,0.));
#6930=DIRECTION('ref_axis',(0.,0.,1.));
#6931=DIRECTION('center_axis',(0.,-1.,0.));
#6932=DIRECTION('ref_axis',(1.,0.,0.));
#6933=DIRECTION('center_axis',(0.,-1.,0.));
#6934=DIRECTION('ref_axis',(1.,0.,0.));
#6935=DIRECTION('center_axis',(0.,-1.,0.));
#6936=DIRECTION('ref_axis',(1.,0.,0.));
#6937=DIRECTION('',(0.,1.,0.));
#6938=DIRECTION('center_axis',(0.,-1.,0.));
#6939=DIRECTION('ref_axis',(0.,0.,-1.));
#6940=DIRECTION('center_axis',(0.,-1.,0.));
#6941=DIRECTION('ref_axis',(1.,0.,0.));
#6942=DIRECTION('center_axis',(0.,-1.,0.));
#6943=DIRECTION('ref_axis',(1.,0.,0.));
#6944=DIRECTION('',(0.,1.,0.));
#6945=DIRECTION('',(0.,0.,1.));
#6946=DIRECTION('',(1.,0.,0.));
#6947=DIRECTION('',(0.,0.,1.));
#6948=DIRECTION('',(1.,0.,0.));
#6949=DIRECTION('axis',(0.,0.,1.));
#6950=DIRECTION('refdir',(1.,0.,0.));
#6951=DIRECTION('center_axis',(0.,1.,0.));
#6952=DIRECTION('ref_axis',(1.,0.,0.));
#6953=DIRECTION('center_axis',(0.,-1.,0.));
#6954=DIRECTION('ref_axis',(1.,0.,0.));
#6955=DIRECTION('',(0.,-1.,0.));
#6956=DIRECTION('center_axis',(0.,-1.,0.));
#6957=DIRECTION('ref_axis',(1.,0.,0.));
#6958=DIRECTION('center_axis',(0.,1.,0.));
#6959=DIRECTION('ref_axis',(1.,0.,0.));
#6960=DIRECTION('center_axis',(0.,1.,0.));
#6961=DIRECTION('ref_axis',(1.,0.,0.));
#6962=DIRECTION('',(0.,-1.,0.));
#6963=DIRECTION('center_axis',(0.,1.,0.));
#6964=DIRECTION('ref_axis',(1.,0.,0.));
#6965=DIRECTION('center_axis',(0.,1.,0.));
#6966=DIRECTION('ref_axis',(1.,0.,0.));
#6967=DIRECTION('center_axis',(0.,1.,0.));
#6968=DIRECTION('ref_axis',(1.,0.,0.));
#6969=DIRECTION('axis',(0.,0.,1.));
#6970=DIRECTION('refdir',(1.,0.,0.));
#6971=DIRECTION('center_axis',(0.866025403784439,0.,-0.5));
#6972=DIRECTION('ref_axis',(0.5,0.,0.866025403784439));
#6973=DIRECTION('',(-0.5,0.,-0.866025403784439));
#6974=DIRECTION('',(0.,-1.,0.));
#6975=DIRECTION('',(0.5,0.,0.866025403784439));
#6976=DIRECTION('',(0.,-1.,0.));
#6977=DIRECTION('center_axis',(1.60246890531964E-16,0.,-1.));
#6978=DIRECTION('ref_axis',(1.,0.,1.60246890531964E-16));
#6979=DIRECTION('',(-1.,0.,-1.60246890531964E-16));
#6980=DIRECTION('',(0.,-1.,0.));
#6981=DIRECTION('',(1.,0.,1.60246890531964E-16));
#6982=DIRECTION('center_axis',(-0.866025403784439,0.,-0.5));
#6983=DIRECTION('ref_axis',(0.5,0.,-0.866025403784439));
#6984=DIRECTION('',(-0.5,0.,0.866025403784439));
#6985=DIRECTION('',(0.,-1.,0.));
#6986=DIRECTION('',(0.5,0.,-0.866025403784439));
#6987=DIRECTION('center_axis',(-0.866025403784439,0.,0.5));
#6988=DIRECTION('ref_axis',(-0.5,0.,-0.866025403784439));
#6989=DIRECTION('',(0.5,0.,0.866025403784439));
#6990=DIRECTION('',(0.,-1.,0.));
#6991=DIRECTION('',(-0.5,0.,-0.866025403784439));
#6992=DIRECTION('center_axis',(-1.60246890531964E-16,0.,1.));
#6993=DIRECTION('ref_axis',(-1.,0.,-1.60246890531964E-16));
#6994=DIRECTION('',(1.,0.,1.60246890531964E-16));
#6995=DIRECTION('',(0.,-1.,0.));
#6996=DIRECTION('',(-1.,0.,-1.60246890531964E-16));
#6997=DIRECTION('center_axis',(0.866025403784439,0.,0.5));
#6998=DIRECTION('ref_axis',(-0.5,0.,0.866025403784439));
#6999=DIRECTION('',(0.5,0.,-0.866025403784439));
#7000=DIRECTION('',(-0.5,0.,0.866025403784439));
#7001=DIRECTION('center_axis',(0.,1.,0.));
#7002=DIRECTION('ref_axis',(1.,0.,0.));
#7003=DIRECTION('center_axis',(0.,-1.,0.));
#7004=DIRECTION('ref_axis',(0.,0.,-1.));
#7005=DIRECTION('center_axis',(0.,1.,0.));
#7006=DIRECTION('ref_axis',(1.,0.,0.));
#7007=DIRECTION('center_axis',(0.,1.,0.));
#7008=DIRECTION('ref_axis',(1.,0.,0.));
#7009=DIRECTION('center_axis',(0.,1.,0.));
#7010=DIRECTION('ref_axis',(0.,0.,1.));
#7011=DIRECTION('center_axis',(0.,-1.,0.));
#7012=DIRECTION('ref_axis',(1.,0.,0.));
#7013=DIRECTION('center_axis',(0.,-1.,0.));
#7014=DIRECTION('ref_axis',(1.,0.,0.));
#7015=DIRECTION('center_axis',(0.,-1.,0.));
#7016=DIRECTION('ref_axis',(1.,0.,0.));
#7017=DIRECTION('',(0.707106781186548,0.707106781186547,8.65956056235493E-17));
#7018=DIRECTION('center_axis',(0.,-1.,0.));
#7019=DIRECTION('ref_axis',(1.,0.,0.));
#7020=DIRECTION('center_axis',(0.,-1.,0.));
#7021=DIRECTION('ref_axis',(1.,0.,0.));
#7022=DIRECTION('',(0.,1.,0.));
#7023=DIRECTION('center_axis',(0.,1.,0.));
#7024=DIRECTION('ref_axis',(1.,0.,0.));
#7025=DIRECTION('center_axis',(0.,-1.,0.));
#7026=DIRECTION('ref_axis',(1.,0.,0.));
#7027=DIRECTION('',(-0.707106781186548,0.707106781186547,-8.65956056235494E-17));
#7028=DIRECTION('center_axis',(0.,-1.,0.));
#7029=DIRECTION('ref_axis',(0.,0.,-1.));
#7030=DIRECTION('center_axis',(0.,-1.,0.));
#7031=DIRECTION('ref_axis',(1.,0.,0.));
#7032=DIRECTION('center_axis',(0.,1.,0.));
#7033=DIRECTION('ref_axis',(1.,0.,0.));
#7034=DIRECTION('center_axis',(0.,1.,0.));
#7035=DIRECTION('ref_axis',(1.,0.,0.));
#7036=DIRECTION('',(-0.447213595499958,0.894427190999916,-5.47678698264203E-17));
#7037=DIRECTION('center_axis',(0.,-1.,0.));
#7038=DIRECTION('ref_axis',(1.,0.,0.));
#7039=DIRECTION('',(0.,1.,0.));
#7040=DIRECTION('',(0.,0.,1.));
#7041=DIRECTION('',(1.,0.,0.));
#7042=DIRECTION('',(0.,0.,1.));
#7043=DIRECTION('',(1.,0.,0.));
#7044=DIRECTION('',(0.,0.,1.));
#7045=DIRECTION('',(1.,0.,0.));
#7046=DIRECTION('',(0.,0.,1.));
#7047=DIRECTION('',(1.,0.,0.));
#7048=DIRECTION('',(0.,0.,1.));
#7049=DIRECTION('',(1.,0.,0.));
#7050=DIRECTION('',(0.,0.,1.));
#7051=DIRECTION('',(1.,0.,0.));
#7052=DIRECTION('',(0.,0.,1.));
#7053=DIRECTION('',(1.,0.,0.));
#7054=DIRECTION('',(0.,0.,1.));
#7055=DIRECTION('',(1.,0.,0.));
#7056=DIRECTION('',(0.,-1.,2.22044604925031E-16));
#7057=DIRECTION('',(1.,0.,0.));
#7058=DIRECTION('',(0.,-1.,2.22044604925031E-16));
#7059=DIRECTION('',(1.,0.,0.));
#7060=DIRECTION('',(0.,-1.,2.22044604925031E-16));
#7061=DIRECTION('',(1.,0.,0.));
#7062=DIRECTION('',(0.,-1.,2.22044604925031E-16));
#7063=DIRECTION('',(1.,0.,0.));
#7064=DIRECTION('',(0.,0.,1.));
#7065=DIRECTION('',(1.,0.,0.));
#7066=DIRECTION('',(0.,-1.,2.22044604925031E-16));
#7067=DIRECTION('',(1.,0.,0.));
#7068=DIRECTION('',(0.,-1.,2.22044604925031E-16));
#7069=DIRECTION('',(1.,0.,0.));
#7070=DIRECTION('',(0.,-1.,2.22044604925031E-16));
#7071=DIRECTION('',(1.,0.,0.));
#7072=DIRECTION('',(0.,-1.,2.22044604925031E-16));
#7073=DIRECTION('',(1.,0.,0.));
#7074=DIRECTION('axis',(0.,0.,1.));
#7075=DIRECTION('refdir',(1.,0.,0.));
#7076=DIRECTION('axis',(0.,0.,1.));
#7077=DIRECTION('refdir',(1.,0.,0.));
#7078=DIRECTION('center_axis',(-1.,0.,0.));
#7079=DIRECTION('ref_axis',(0.,0.,1.));
#7080=DIRECTION('',(0.,-1.,0.));
#7081=DIRECTION('',(0.,0.,1.));
#7082=DIRECTION('',(0.,1.,0.));
#7083=DIRECTION('',(0.,0.,-1.));
#7084=DIRECTION('center_axis',(0.,1.,0.));
#7085=DIRECTION('ref_axis',(1.,0.,0.));
#7086=DIRECTION('center_axis',(0.,-1.,0.));
#7087=DIRECTION('ref_axis',(1.,0.,0.));
#7088=DIRECTION('',(-1.,0.,0.));
#7089=DIRECTION('',(0.,0.,1.));
#7090=DIRECTION('center_axis',(1.,0.,0.));
#7091=DIRECTION('ref_axis',(0.,0.,-1.));
#7092=DIRECTION('',(0.,1.,0.));
#7093=DIRECTION('',(0.,1.,0.));
#7094=DIRECTION('',(0.,0.,-1.));
#7095=DIRECTION('center_axis',(0.,0.,1.));
#7096=DIRECTION('ref_axis',(1.,0.,0.));
#7097=DIRECTION('',(1.,0.,0.));
#7098=DIRECTION('center_axis',(0.,1.,0.));
#7099=DIRECTION('ref_axis',(0.,0.,1.));
#7100=DIRECTION('center_axis',(0.,1.,0.));
#7101=DIRECTION('ref_axis',(1.,0.,0.));
#7102=DIRECTION('center_axis',(0.,1.,0.));
#7103=DIRECTION('ref_axis',(1.,0.,0.));
#7104=DIRECTION('center_axis',(0.,1.,0.));
#7105=DIRECTION('ref_axis',(1.,0.,0.));
#7106=DIRECTION('',(0.,1.,0.));
#7107=DIRECTION('center_axis',(0.,-1.,0.));
#7108=DIRECTION('ref_axis',(1.,0.,0.));
#7109=DIRECTION('center_axis',(0.,1.,0.));
#7110=DIRECTION('ref_axis',(1.,0.,0.));
#7111=DIRECTION('center_axis',(0.,1.,0.));
#7112=DIRECTION('ref_axis',(1.,0.,0.));
#7113=DIRECTION('center_axis',(0.,1.,0.));
#7114=DIRECTION('ref_axis',(1.,0.,0.));
#7115=DIRECTION('',(0.,1.,0.));
#7116=DIRECTION('center_axis',(0.,1.,0.));
#7117=DIRECTION('ref_axis',(1.,0.,0.));
#7118=DIRECTION('center_axis',(0.,1.,0.));
#7119=DIRECTION('ref_axis',(1.,0.,0.));
#7120=DIRECTION('center_axis',(-1.,0.,0.));
#7121=DIRECTION('ref_axis',(0.,0.,1.));
#7122=DIRECTION('',(0.,-1.,0.));
#7123=DIRECTION('',(0.,0.,1.));
#7124=DIRECTION('',(0.,1.,0.));
#7125=DIRECTION('',(0.,0.,-1.));
#7126=DIRECTION('center_axis',(0.,1.,0.));
#7127=DIRECTION('ref_axis',(1.,0.,0.));
#7128=DIRECTION('center_axis',(0.,-1.,0.));
#7129=DIRECTION('ref_axis',(1.,0.,0.));
#7130=DIRECTION('',(-1.,0.,0.));
#7131=DIRECTION('',(0.,0.,1.));
#7132=DIRECTION('center_axis',(1.,0.,0.));
#7133=DIRECTION('ref_axis',(0.,0.,-1.));
#7134=DIRECTION('',(0.,1.,0.));
#7135=DIRECTION('',(0.,1.,0.));
#7136=DIRECTION('',(0.,0.,-1.));
#7137=DIRECTION('center_axis',(0.,0.,1.));
#7138=DIRECTION('ref_axis',(1.,0.,0.));
#7139=DIRECTION('',(1.,0.,0.));
#7140=DIRECTION('center_axis',(0.,1.,0.));
#7141=DIRECTION('ref_axis',(0.,0.,1.));
#7142=DIRECTION('center_axis',(0.,1.,0.));
#7143=DIRECTION('ref_axis',(1.,0.,0.));
#7144=DIRECTION('center_axis',(-1.,0.,0.));
#7145=DIRECTION('ref_axis',(0.,0.,1.));
#7146=DIRECTION('',(0.,-1.,0.));
#7147=DIRECTION('',(0.,0.,1.));
#7148=DIRECTION('',(0.,1.,0.));
#7149=DIRECTION('',(0.,0.,-1.));
#7150=DIRECTION('center_axis',(0.,1.,0.));
#7151=DIRECTION('ref_axis',(1.,0.,0.));
#7152=DIRECTION('center_axis',(0.,-1.,0.));
#7153=DIRECTION('ref_axis',(1.,0.,0.));
#7154=DIRECTION('',(-1.,0.,0.));
#7155=DIRECTION('',(0.,0.,1.));
#7156=DIRECTION('center_axis',(1.,0.,0.));
#7157=DIRECTION('ref_axis',(0.,0.,-1.));
#7158=DIRECTION('',(0.,1.,0.));
#7159=DIRECTION('',(0.,1.,0.));
#7160=DIRECTION('',(0.,0.,-1.));
#7161=DIRECTION('center_axis',(0.,0.,1.));
#7162=DIRECTION('ref_axis',(1.,0.,0.));
#7163=DIRECTION('',(1.,0.,0.));
#7164=DIRECTION('center_axis',(0.,1.,0.));
#7165=DIRECTION('ref_axis',(0.,0.,1.));
#7166=DIRECTION('center_axis',(0.,1.,0.));
#7167=DIRECTION('ref_axis',(1.,0.,0.));
#7168=DIRECTION('center_axis',(0.,1.,0.));
#7169=DIRECTION('ref_axis',(1.,0.,0.));
#7170=DIRECTION('center_axis',(0.,1.,0.));
#7171=DIRECTION('ref_axis',(1.,0.,0.));
#7172=DIRECTION('',(0.,-1.,0.));
#7173=DIRECTION('center_axis',(0.,-1.,0.));
#7174=DIRECTION('ref_axis',(1.,0.,0.));
#7175=DIRECTION('center_axis',(0.,1.,0.));
#7176=DIRECTION('ref_axis',(1.,0.,0.));
#7177=DIRECTION('center_axis',(0.,1.,0.));
#7178=DIRECTION('ref_axis',(1.,0.,0.));
#7179=DIRECTION('center_axis',(0.,1.,0.));
#7180=DIRECTION('ref_axis',(1.,0.,0.));
#7181=DIRECTION('',(0.,-1.,0.));
#7182=DIRECTION('center_axis',(0.,1.,0.));
#7183=DIRECTION('ref_axis',(1.,0.,0.));
#7184=DIRECTION('center_axis',(0.,1.,0.));
#7185=DIRECTION('ref_axis',(1.,0.,0.));
#7186=DIRECTION('center_axis',(0.,1.,0.));
#7187=DIRECTION('ref_axis',(1.,0.,0.));
#7188=DIRECTION('center_axis',(0.,1.,0.));
#7189=DIRECTION('ref_axis',(1.,0.,0.));
#7190=DIRECTION('',(0.,-1.,0.));
#7191=DIRECTION('center_axis',(0.,1.,0.));
#7192=DIRECTION('ref_axis',(1.,0.,0.));
#7193=DIRECTION('center_axis',(0.,1.,0.));
#7194=DIRECTION('ref_axis',(1.,0.,0.));
#7195=DIRECTION('center_axis',(0.,1.,0.));
#7196=DIRECTION('ref_axis',(1.,0.,0.));
#7197=DIRECTION('axis',(0.,0.,1.));
#7198=DIRECTION('refdir',(1.,0.,0.));
#7199=DIRECTION('center_axis',(0.,1.,0.));
#7200=DIRECTION('ref_axis',(1.,0.,0.));
#7201=DIRECTION('center_axis',(0.,-1.,0.));
#7202=DIRECTION('ref_axis',(1.,0.,0.));
#7203=DIRECTION('',(0.,-1.,0.));
#7204=DIRECTION('center_axis',(0.,-1.,0.));
#7205=DIRECTION('ref_axis',(1.,0.,0.));
#7206=DIRECTION('center_axis',(0.,1.,0.));
#7207=DIRECTION('ref_axis',(1.,0.,0.));
#7208=DIRECTION('center_axis',(0.,1.,0.));
#7209=DIRECTION('ref_axis',(1.,0.,0.));
#7210=DIRECTION('',(0.,-1.,0.));
#7211=DIRECTION('center_axis',(0.,1.,0.));
#7212=DIRECTION('ref_axis',(1.,0.,0.));
#7213=DIRECTION('center_axis',(0.,1.,0.));
#7214=DIRECTION('ref_axis',(1.,0.,0.));
#7215=DIRECTION('center_axis',(0.,1.,0.));
#7216=DIRECTION('ref_axis',(1.,0.,0.));
#7217=DIRECTION('axis',(0.,0.,1.));
#7218=DIRECTION('refdir',(1.,0.,0.));
#7219=DIRECTION('center_axis',(0.,1.,0.));
#7220=DIRECTION('ref_axis',(1.,0.,0.));
#7221=DIRECTION('center_axis',(0.,-1.,0.));
#7222=DIRECTION('ref_axis',(1.,0.,0.));
#7223=DIRECTION('',(0.,-1.,0.));
#7224=DIRECTION('center_axis',(0.,-1.,0.));
#7225=DIRECTION('ref_axis',(1.,0.,0.));
#7226=DIRECTION('center_axis',(0.,1.,0.));
#7227=DIRECTION('ref_axis',(1.,0.,0.));
#7228=DIRECTION('center_axis',(0.,1.,0.));
#7229=DIRECTION('ref_axis',(1.,0.,0.));
#7230=DIRECTION('',(0.,-1.,0.));
#7231=DIRECTION('center_axis',(0.,1.,0.));
#7232=DIRECTION('ref_axis',(1.,0.,0.));
#7233=DIRECTION('center_axis',(0.,1.,0.));
#7234=DIRECTION('ref_axis',(1.,0.,0.));
#7235=DIRECTION('center_axis',(0.,1.,0.));
#7236=DIRECTION('ref_axis',(1.,0.,0.));
#7237=DIRECTION('axis',(0.,0.,1.));
#7238=DIRECTION('refdir',(1.,0.,0.));
#7239=DIRECTION('center_axis',(0.,1.,0.));
#7240=DIRECTION('ref_axis',(1.,0.,0.));
#7241=DIRECTION('center_axis',(0.,-1.,0.));
#7242=DIRECTION('ref_axis',(1.,0.,0.));
#7243=DIRECTION('',(0.,-1.,0.));
#7244=DIRECTION('center_axis',(0.,-1.,0.));
#7245=DIRECTION('ref_axis',(1.,0.,0.));
#7246=DIRECTION('center_axis',(0.,1.,0.));
#7247=DIRECTION('ref_axis',(1.,0.,0.));
#7248=DIRECTION('center_axis',(0.,1.,0.));
#7249=DIRECTION('ref_axis',(1.,0.,0.));
#7250=DIRECTION('',(0.,-1.,0.));
#7251=DIRECTION('center_axis',(0.,1.,0.));
#7252=DIRECTION('ref_axis',(1.,0.,0.));
#7253=DIRECTION('center_axis',(0.,1.,0.));
#7254=DIRECTION('ref_axis',(1.,0.,0.));
#7255=DIRECTION('center_axis',(0.,1.,0.));
#7256=DIRECTION('ref_axis',(1.,0.,0.));
#7257=DIRECTION('axis',(0.,0.,1.));
#7258=DIRECTION('refdir',(1.,0.,0.));
#7259=DIRECTION('center_axis',(0.,1.,0.));
#7260=DIRECTION('ref_axis',(1.,0.,0.));
#7261=DIRECTION('center_axis',(0.,-1.,0.));
#7262=DIRECTION('ref_axis',(1.,0.,0.));
#7263=DIRECTION('',(0.,-1.,0.));
#7264=DIRECTION('center_axis',(0.,-1.,0.));
#7265=DIRECTION('ref_axis',(1.,0.,0.));
#7266=DIRECTION('center_axis',(0.,1.,0.));
#7267=DIRECTION('ref_axis',(1.,0.,0.));
#7268=DIRECTION('center_axis',(0.,1.,0.));
#7269=DIRECTION('ref_axis',(1.,0.,0.));
#7270=DIRECTION('',(0.,-1.,0.));
#7271=DIRECTION('center_axis',(0.,1.,0.));
#7272=DIRECTION('ref_axis',(1.,0.,0.));
#7273=DIRECTION('center_axis',(0.,1.,0.));
#7274=DIRECTION('ref_axis',(1.,0.,0.));
#7275=DIRECTION('center_axis',(0.,1.,0.));
#7276=DIRECTION('ref_axis',(1.,0.,0.));
#7277=DIRECTION('axis',(0.,0.,1.));
#7278=DIRECTION('refdir',(1.,0.,0.));
#7279=DIRECTION('center_axis',(0.,1.,0.));
#7280=DIRECTION('ref_axis',(1.,0.,0.));
#7281=DIRECTION('center_axis',(0.,-1.,0.));
#7282=DIRECTION('ref_axis',(1.,0.,0.));
#7283=DIRECTION('',(0.,-1.,0.));
#7284=DIRECTION('center_axis',(0.,-1.,0.));
#7285=DIRECTION('ref_axis',(1.,0.,0.));
#7286=DIRECTION('center_axis',(0.,1.,0.));
#7287=DIRECTION('ref_axis',(1.,0.,0.));
#7288=DIRECTION('center_axis',(0.,1.,0.));
#7289=DIRECTION('ref_axis',(1.,0.,0.));
#7290=DIRECTION('',(0.,-1.,0.));
#7291=DIRECTION('center_axis',(0.,1.,0.));
#7292=DIRECTION('ref_axis',(1.,0.,0.));
#7293=DIRECTION('center_axis',(0.,1.,0.));
#7294=DIRECTION('ref_axis',(1.,0.,0.));
#7295=DIRECTION('center_axis',(0.,1.,0.));
#7296=DIRECTION('ref_axis',(1.,0.,0.));
#7297=DIRECTION('axis',(0.,0.,1.));
#7298=DIRECTION('refdir',(1.,0.,0.));
#7299=DIRECTION('center_axis',(0.,0.,1.));
#7300=DIRECTION('ref_axis',(1.,0.,0.));
#7301=DIRECTION('',(0.,1.,0.));
#7302=DIRECTION('center_axis',(0.,0.,1.));
#7303=DIRECTION('ref_axis',(1.,0.,0.));
#7304=DIRECTION('center_axis',(0.,0.,1.));
#7305=DIRECTION('ref_axis',(1.,0.,0.));
#7306=DIRECTION('center_axis',(0.,0.,1.));
#7307=DIRECTION('ref_axis',(1.,0.,0.));
#7308=DIRECTION('',(0.,0.,1.));
#7309=DIRECTION('center_axis',(0.,0.,1.));
#7310=DIRECTION('ref_axis',(1.,0.,0.));
#7311=DIRECTION('center_axis',(0.,0.,1.));
#7312=DIRECTION('ref_axis',(1.,0.,0.));
#7313=DIRECTION('',(0.,-1.,0.));
#7314=DIRECTION('center_axis',(-1.,0.,0.));
#7315=DIRECTION('ref_axis',(0.,0.,1.));
#7316=DIRECTION('',(0.,0.,1.));
#7317=DIRECTION('',(0.,1.,0.));
#7318=DIRECTION('',(0.,0.,-1.));
#7319=DIRECTION('',(0.,1.,0.));
#7320=DIRECTION('center_axis',(0.,0.,-1.));
#7321=DIRECTION('ref_axis',(-1.,0.,0.));
#7322=DIRECTION('',(-1.,0.,0.));
#7323=DIRECTION('',(0.,1.,0.));
#7324=DIRECTION('',(1.,0.,0.));
#7325=DIRECTION('center_axis',(1.,0.,0.));
#7326=DIRECTION('ref_axis',(0.,0.,-1.));
#7327=DIRECTION('',(0.,0.,-1.));
#7328=DIRECTION('',(0.,-1.,0.));
#7329=DIRECTION('',(0.,0.,1.));
#7330=DIRECTION('center_axis',(0.,1.,0.));
#7331=DIRECTION('ref_axis',(1.,0.,0.));
#7332=DIRECTION('center_axis',(0.,1.,0.));
#7333=DIRECTION('ref_axis',(1.,0.,0.));
#7334=DIRECTION('center_axis',(0.,-1.,0.));
#7335=DIRECTION('ref_axis',(1.,0.,0.));
#7336=DIRECTION('center_axis',(0.,1.,0.));
#7337=DIRECTION('ref_axis',(-1.83697019872103E-16,0.,1.));
#7338=DIRECTION('center_axis',(0.,-1.,0.));
#7339=DIRECTION('ref_axis',(1.,0.,0.));
#7340=DIRECTION('center_axis',(0.,1.,0.));
#7341=DIRECTION('ref_axis',(1.,0.,0.));
#7342=DIRECTION('',(0.,-1.,0.));
#7343=DIRECTION('center_axis',(0.,1.,0.));
#7344=DIRECTION('ref_axis',(1.,0.,0.));
#7345=DIRECTION('center_axis',(0.,1.,0.));
#7346=DIRECTION('ref_axis',(1.,0.,0.));
#7347=DIRECTION('axis',(0.,0.,1.));
#7348=DIRECTION('refdir',(1.,0.,0.));
#7349=DIRECTION('center_axis',(0.,0.,1.));
#7350=DIRECTION('ref_axis',(1.,0.,0.));
#7351=DIRECTION('',(0.,1.,0.));
#7352=DIRECTION('center_axis',(0.,0.,1.));
#7353=DIRECTION('ref_axis',(1.,0.,0.));
#7354=DIRECTION('center_axis',(0.,0.,1.));
#7355=DIRECTION('ref_axis',(1.,0.,0.));
#7356=DIRECTION('center_axis',(0.,0.,1.));
#7357=DIRECTION('ref_axis',(1.,0.,0.));
#7358=DIRECTION('',(0.,0.,1.));
#7359=DIRECTION('center_axis',(0.,0.,1.));
#7360=DIRECTION('ref_axis',(1.,0.,0.));
#7361=DIRECTION('center_axis',(0.,0.,1.));
#7362=DIRECTION('ref_axis',(1.,0.,0.));
#7363=DIRECTION('',(0.,-1.,0.));
#7364=DIRECTION('center_axis',(0.,1.,0.));
#7365=DIRECTION('ref_axis',(1.,0.,0.));
#7366=DIRECTION('center_axis',(0.,-1.,0.));
#7367=DIRECTION('ref_axis',(1.,0.,0.));
#7368=DIRECTION('',(0.,-1.,0.));
#7369=DIRECTION('center_axis',(0.,-1.,0.));
#7370=DIRECTION('ref_axis',(1.,0.,0.));
#7371=DIRECTION('center_axis',(0.,1.,0.));
#7372=DIRECTION('ref_axis',(1.,0.,0.));
#7373=DIRECTION('center_axis',(0.,1.,0.));
#7374=DIRECTION('ref_axis',(1.,0.,0.));
#7375=DIRECTION('',(0.,-1.,0.));
#7376=DIRECTION('center_axis',(0.,1.,0.));
#7377=DIRECTION('ref_axis',(1.,0.,0.));
#7378=DIRECTION('center_axis',(0.,1.,0.));
#7379=DIRECTION('ref_axis',(1.,0.,0.));
#7380=DIRECTION('center_axis',(0.,1.,0.));
#7381=DIRECTION('ref_axis',(1.,0.,0.));
#7382=DIRECTION('axis',(0.,0.,1.));
#7383=DIRECTION('refdir',(1.,0.,0.));
#7384=DIRECTION('center_axis',(0.,0.,1.));
#7385=DIRECTION('ref_axis',(1.,0.,0.));
#7386=DIRECTION('',(0.,1.,0.));
#7387=DIRECTION('center_axis',(0.,0.,1.));
#7388=DIRECTION('ref_axis',(1.,0.,0.));
#7389=DIRECTION('center_axis',(0.,0.,1.));
#7390=DIRECTION('ref_axis',(1.,0.,0.));
#7391=DIRECTION('center_axis',(0.,0.,1.));
#7392=DIRECTION('ref_axis',(1.,0.,0.));
#7393=DIRECTION('',(0.,0.,1.));
#7394=DIRECTION('center_axis',(0.,0.,1.));
#7395=DIRECTION('ref_axis',(1.,0.,0.));
#7396=DIRECTION('center_axis',(0.,0.,1.));
#7397=DIRECTION('ref_axis',(1.,0.,0.));
#7398=DIRECTION('',(0.,-1.,0.));
#7399=DIRECTION('center_axis',(0.,1.,0.));
#7400=DIRECTION('ref_axis',(1.,0.,0.));
#7401=DIRECTION('center_axis',(0.,-1.,0.));
#7402=DIRECTION('ref_axis',(1.,0.,0.));
#7403=DIRECTION('',(0.,-1.,0.));
#7404=DIRECTION('center_axis',(0.,-1.,0.));
#7405=DIRECTION('ref_axis',(1.,0.,0.));
#7406=DIRECTION('center_axis',(0.,1.,0.));
#7407=DIRECTION('ref_axis',(1.,0.,0.));
#7408=DIRECTION('center_axis',(0.,1.,0.));
#7409=DIRECTION('ref_axis',(1.,0.,0.));
#7410=DIRECTION('',(0.,-1.,0.));
#7411=DIRECTION('center_axis',(0.,1.,0.));
#7412=DIRECTION('ref_axis',(1.,0.,0.));
#7413=DIRECTION('center_axis',(0.,1.,0.));
#7414=DIRECTION('ref_axis',(1.,0.,0.));
#7415=DIRECTION('center_axis',(0.,1.,0.));
#7416=DIRECTION('ref_axis',(1.,0.,0.));
#7417=DIRECTION('axis',(0.,0.,1.));
#7418=DIRECTION('refdir',(1.,0.,0.));
#7419=DIRECTION('center_axis',(-1.,0.,0.));
#7420=DIRECTION('ref_axis',(0.,0.,1.));
#7421=DIRECTION('',(0.,0.,1.));
#7422=DIRECTION('',(0.,1.,0.));
#7423=DIRECTION('',(0.,0.,-1.));
#7424=DIRECTION('',(0.,1.,0.));
#7425=DIRECTION('center_axis',(0.,0.,-1.));
#7426=DIRECTION('ref_axis',(-1.,0.,0.));
#7427=DIRECTION('',(-1.,0.,0.));
#7428=DIRECTION('',(0.,1.,0.));
#7429=DIRECTION('',(1.,0.,0.));
#7430=DIRECTION('center_axis',(0.,0.,1.));
#7431=DIRECTION('ref_axis',(1.,0.,0.));
#7432=DIRECTION('center_axis',(1.,0.,0.));
#7433=DIRECTION('ref_axis',(0.,0.,-1.));
#7434=DIRECTION('',(0.,0.,-1.));
#7435=DIRECTION('',(0.,-1.,0.));
#7436=DIRECTION('',(0.,0.,1.));
#7437=DIRECTION('center_axis',(0.,1.,0.));
#7438=DIRECTION('ref_axis',(1.,0.,0.));
#7439=DIRECTION('center_axis',(0.,1.,0.));
#7440=DIRECTION('ref_axis',(1.,0.,0.));
#7441=DIRECTION('center_axis',(0.,-1.,0.));
#7442=DIRECTION('ref_axis',(1.,0.,0.));
#7443=DIRECTION('center_axis',(0.,1.,0.));
#7444=DIRECTION('ref_axis',(-1.83697019872103E-16,0.,1.));
#7445=DIRECTION('center_axis',(0.,1.,0.));
#7446=DIRECTION('ref_axis',(1.,0.,0.));
#7447=DIRECTION('center_axis',(1.,0.,6.12323399573677E-17));
#7448=DIRECTION('ref_axis',(6.12323399573677E-17,0.,-1.));
#7449=DIRECTION('',(1.,0.,6.12323399573677E-17));
#7450=DIRECTION('center_axis',(1.,0.,6.12323399573677E-17));
#7451=DIRECTION('ref_axis',(6.12323399573677E-17,0.,-1.));
#7452=DIRECTION('',(1.,0.,6.12323399573677E-17));
#7453=DIRECTION('center_axis',(0.,-1.,0.));
#7454=DIRECTION('ref_axis',(1.,0.,0.));
#7455=DIRECTION('center_axis',(0.,-1.,0.));
#7456=DIRECTION('ref_axis',(1.,0.,0.));
#7457=DIRECTION('',(0.,1.,0.));
#7458=DIRECTION('',(0.,1.,0.));
#7459=DIRECTION('center_axis',(0.,1.,0.));
#7460=DIRECTION('ref_axis',(1.,0.,0.));
#7461=DIRECTION('center_axis',(0.,0.,1.));
#7462=DIRECTION('ref_axis',(1.,0.,0.));
#7463=DIRECTION('',(0.,0.,1.));
#7464=DIRECTION('center_axis',(0.,0.,1.));
#7465=DIRECTION('ref_axis',(1.,0.,0.));
#7466=DIRECTION('',(0.,0.,1.));
#7467=DIRECTION('center_axis',(0.,1.,0.));
#7468=DIRECTION('ref_axis',(1.,0.,0.));
#7469=DIRECTION('center_axis',(0.,1.,0.));
#7470=DIRECTION('ref_axis',(1.,0.,0.));
#7471=DIRECTION('center_axis',(0.,1.,0.));
#7472=DIRECTION('ref_axis',(1.,0.,0.));
#7473=DIRECTION('center_axis',(0.,1.,0.));
#7474=DIRECTION('ref_axis',(0.987688340595138,0.,0.156434465040231));
#7475=DIRECTION('center_axis',(0.,1.,0.));
#7476=DIRECTION('ref_axis',(1.,0.,0.));
#7477=DIRECTION('center_axis',(0.,1.,0.));
#7478=DIRECTION('ref_axis',(0.951056516295154,0.,0.309016994374948));
#7479=DIRECTION('center_axis',(0.,1.,0.));
#7480=DIRECTION('ref_axis',(1.,0.,0.));
#7481=DIRECTION('center_axis',(0.,1.,0.));
#7482=DIRECTION('ref_axis',(0.891006524188368,0.,0.453990499739547));
#7483=DIRECTION('center_axis',(0.,1.,0.));
#7484=DIRECTION('ref_axis',(1.,0.,0.));
#7485=DIRECTION('center_axis',(0.,1.,0.));
#7486=DIRECTION('ref_axis',(0.809016994374947,0.,0.587785252292473));
#7487=DIRECTION('center_axis',(0.,1.,0.));
#7488=DIRECTION('ref_axis',(1.,0.,0.));
#7489=DIRECTION('center_axis',(0.,1.,0.));
#7490=DIRECTION('ref_axis',(0.707106781186547,0.,0.707106781186548));
#7491=DIRECTION('center_axis',(0.,1.,0.));
#7492=DIRECTION('ref_axis',(1.,0.,0.));
#7493=DIRECTION('center_axis',(0.,1.,0.));
#7494=DIRECTION('ref_axis',(0.587785252292473,0.,0.809016994374948));
#7495=DIRECTION('center_axis',(0.,1.,0.));
#7496=DIRECTION('ref_axis',(1.,0.,0.));
#7497=DIRECTION('center_axis',(0.,1.,0.));
#7498=DIRECTION('ref_axis',(0.453990499739547,0.,0.891006524188368));
#7499=DIRECTION('center_axis',(0.,1.,0.));
#7500=DIRECTION('ref_axis',(1.,0.,0.));
#7501=DIRECTION('center_axis',(0.,1.,0.));
#7502=DIRECTION('ref_axis',(0.309016994374947,0.,0.951056516295154));
#7503=DIRECTION('center_axis',(0.,1.,0.));
#7504=DIRECTION('ref_axis',(1.,0.,0.));
#7505=DIRECTION('center_axis',(0.,1.,0.));
#7506=DIRECTION('ref_axis',(0.156434465040231,0.,0.987688340595138));
#7507=DIRECTION('center_axis',(0.,1.,0.));
#7508=DIRECTION('ref_axis',(1.,0.,0.));
#7509=DIRECTION('center_axis',(0.,1.,0.));
#7510=DIRECTION('ref_axis',(-1.83697019872103E-16,0.,1.));
#7511=DIRECTION('center_axis',(0.,1.,0.));
#7512=DIRECTION('ref_axis',(1.,0.,0.));
#7513=DIRECTION('center_axis',(0.,1.,0.));
#7514=DIRECTION('ref_axis',(-0.156434465040231,0.,0.987688340595138));
#7515=DIRECTION('center_axis',(0.,1.,0.));
#7516=DIRECTION('ref_axis',(1.,0.,0.));
#7517=DIRECTION('center_axis',(0.,1.,0.));
#7518=DIRECTION('ref_axis',(-0.309016994374948,0.,0.951056516295154));
#7519=DIRECTION('center_axis',(0.,1.,0.));
#7520=DIRECTION('ref_axis',(1.,0.,0.));
#7521=DIRECTION('center_axis',(0.,1.,0.));
#7522=DIRECTION('ref_axis',(-0.453990499739547,0.,0.891006524188368));
#7523=DIRECTION('center_axis',(0.,1.,0.));
#7524=DIRECTION('ref_axis',(1.,0.,0.));
#7525=DIRECTION('center_axis',(0.,1.,0.));
#7526=DIRECTION('ref_axis',(-0.587785252292473,0.,0.809016994374947));
#7527=DIRECTION('center_axis',(0.,1.,0.));
#7528=DIRECTION('ref_axis',(1.,0.,0.));
#7529=DIRECTION('center_axis',(0.,1.,0.));
#7530=DIRECTION('ref_axis',(-0.707106781186548,0.,0.707106781186547));
#7531=DIRECTION('center_axis',(0.,1.,0.));
#7532=DIRECTION('ref_axis',(1.,0.,0.));
#7533=DIRECTION('center_axis',(0.,1.,0.));
#7534=DIRECTION('ref_axis',(-0.809016994374947,0.,0.587785252292473));
#7535=DIRECTION('center_axis',(0.,1.,0.));
#7536=DIRECTION('ref_axis',(1.,0.,0.));
#7537=DIRECTION('center_axis',(0.,1.,0.));
#7538=DIRECTION('ref_axis',(-0.891006524188368,0.,0.453990499739547));
#7539=DIRECTION('center_axis',(0.,1.,0.));
#7540=DIRECTION('ref_axis',(1.,0.,0.));
#7541=DIRECTION('center_axis',(0.,1.,0.));
#7542=DIRECTION('ref_axis',(-0.951056516295154,0.,0.309016994374947));
#7543=DIRECTION('center_axis',(0.,1.,0.));
#7544=DIRECTION('ref_axis',(1.,0.,0.));
#7545=DIRECTION('center_axis',(0.,1.,0.));
#7546=DIRECTION('ref_axis',(-0.987688340595138,0.,0.156434465040231));
#7547=DIRECTION('center_axis',(0.,1.,0.));
#7548=DIRECTION('ref_axis',(1.,0.,0.));
#7549=DIRECTION('center_axis',(0.,1.,0.));
#7550=DIRECTION('ref_axis',(-1.,0.,-1.22464679914735E-16));
#7551=DIRECTION('center_axis',(0.,1.,0.));
#7552=DIRECTION('ref_axis',(1.,0.,0.));
#7553=DIRECTION('center_axis',(0.,1.,0.));
#7554=DIRECTION('ref_axis',(-0.987688340595138,0.,-0.156434465040231));
#7555=DIRECTION('center_axis',(0.,1.,0.));
#7556=DIRECTION('ref_axis',(1.,0.,0.));
#7557=DIRECTION('center_axis',(0.,1.,0.));
#7558=DIRECTION('ref_axis',(-0.951056516295154,0.,-0.309016994374948));
#7559=DIRECTION('center_axis',(0.,1.,0.));
#7560=DIRECTION('ref_axis',(1.,0.,0.));
#7561=DIRECTION('center_axis',(0.,1.,0.));
#7562=DIRECTION('ref_axis',(-0.891006524188368,0.,-0.453990499739547));
#7563=DIRECTION('center_axis',(0.,1.,0.));
#7564=DIRECTION('ref_axis',(1.,0.,0.));
#7565=DIRECTION('center_axis',(0.,1.,0.));
#7566=DIRECTION('ref_axis',(-0.809016994374947,0.,-0.587785252292473));
#7567=DIRECTION('center_axis',(0.,1.,0.));
#7568=DIRECTION('ref_axis',(1.,0.,0.));
#7569=DIRECTION('center_axis',(0.,1.,0.));
#7570=DIRECTION('ref_axis',(-0.707106781186547,0.,-0.707106781186548));
#7571=DIRECTION('center_axis',(0.,1.,0.));
#7572=DIRECTION('ref_axis',(1.,0.,0.));
#7573=DIRECTION('center_axis',(0.,1.,0.));
#7574=DIRECTION('ref_axis',(-0.587785252292473,0.,-0.809016994374947));
#7575=DIRECTION('center_axis',(0.,1.,0.));
#7576=DIRECTION('ref_axis',(1.,0.,0.));
#7577=DIRECTION('center_axis',(0.,1.,0.));
#7578=DIRECTION('ref_axis',(-0.453990499739547,0.,-0.891006524188368));
#7579=DIRECTION('center_axis',(0.,1.,0.));
#7580=DIRECTION('ref_axis',(1.,0.,0.));
#7581=DIRECTION('center_axis',(0.,1.,0.));
#7582=DIRECTION('ref_axis',(-0.309016994374947,0.,-0.951056516295154));
#7583=DIRECTION('center_axis',(0.,1.,0.));
#7584=DIRECTION('ref_axis',(1.,0.,0.));
#7585=DIRECTION('center_axis',(0.,1.,0.));
#7586=DIRECTION('ref_axis',(-0.156434465040231,0.,-0.987688340595138));
#7587=DIRECTION('center_axis',(0.,1.,0.));
#7588=DIRECTION('ref_axis',(1.,0.,0.));
#7589=DIRECTION('center_axis',(0.,1.,0.));
#7590=DIRECTION('ref_axis',(6.12323399573677E-17,0.,-1.));
#7591=DIRECTION('center_axis',(0.,1.,0.));
#7592=DIRECTION('ref_axis',(1.,0.,0.));
#7593=DIRECTION('center_axis',(0.,1.,0.));
#7594=DIRECTION('ref_axis',(0.156434465040231,0.,-0.987688340595138));
#7595=DIRECTION('center_axis',(0.,1.,0.));
#7596=DIRECTION('ref_axis',(1.,0.,0.));
#7597=DIRECTION('center_axis',(0.,1.,0.));
#7598=DIRECTION('ref_axis',(0.309016994374948,0.,-0.951056516295154));
#7599=DIRECTION('center_axis',(0.,1.,0.));
#7600=DIRECTION('ref_axis',(1.,0.,0.));
#7601=DIRECTION('center_axis',(0.,1.,0.));
#7602=DIRECTION('ref_axis',(0.453990499739547,0.,-0.891006524188368));
#7603=DIRECTION('center_axis',(0.,1.,0.));
#7604=DIRECTION('ref_axis',(1.,0.,0.));
#7605=DIRECTION('center_axis',(0.,1.,0.));
#7606=DIRECTION('ref_axis',(0.587785252292473,0.,-0.809016994374947));
#7607=DIRECTION('center_axis',(0.,1.,0.));
#7608=DIRECTION('ref_axis',(1.,0.,0.));
#7609=DIRECTION('center_axis',(0.,1.,0.));
#7610=DIRECTION('ref_axis',(0.707106781186548,0.,-0.707106781186547));
#7611=DIRECTION('center_axis',(0.,1.,0.));
#7612=DIRECTION('ref_axis',(1.,0.,0.));
#7613=DIRECTION('center_axis',(0.,1.,0.));
#7614=DIRECTION('ref_axis',(0.809016994374947,0.,-0.587785252292473));
#7615=DIRECTION('center_axis',(0.,1.,0.));
#7616=DIRECTION('ref_axis',(1.,0.,0.));
#7617=DIRECTION('center_axis',(0.,1.,0.));
#7618=DIRECTION('ref_axis',(0.891006524188368,0.,-0.453990499739547));
#7619=DIRECTION('center_axis',(0.,1.,0.));
#7620=DIRECTION('ref_axis',(1.,0.,0.));
#7621=DIRECTION('center_axis',(0.,1.,0.));
#7622=DIRECTION('ref_axis',(0.951056516295154,0.,-0.309016994374947));
#7623=DIRECTION('center_axis',(0.,1.,0.));
#7624=DIRECTION('ref_axis',(1.,0.,0.));
#7625=DIRECTION('center_axis',(0.,1.,0.));
#7626=DIRECTION('ref_axis',(0.987688340595138,0.,-0.156434465040231));
#7627=DIRECTION('center_axis',(0.,1.,0.));
#7628=DIRECTION('ref_axis',(1.,0.,0.));
#7629=DIRECTION('center_axis',(0.,1.,0.));
#7630=DIRECTION('ref_axis',(1.,0.,0.));
#7631=DIRECTION('center_axis',(0.,1.,0.));
#7632=DIRECTION('ref_axis',(1.,0.,0.));
#7633=DIRECTION('center_axis',(0.,-1.,0.));
#7634=DIRECTION('ref_axis',(1.,0.,0.));
#7635=DIRECTION('center_axis',(0.,-1.,0.));
#7636=DIRECTION('ref_axis',(1.,0.,0.));
#7637=DIRECTION('',(0.,1.,0.));
#7638=DIRECTION('center_axis',(0.,1.,0.));
#7639=DIRECTION('ref_axis',(1.,0.,0.));
#7640=DIRECTION('center_axis',(0.,1.,0.));
#7641=DIRECTION('ref_axis',(1.,0.,0.));
#7642=DIRECTION('center_axis',(0.,1.,0.));
#7643=DIRECTION('ref_axis',(1.,0.,0.));
#7644=DIRECTION('center_axis',(0.,-1.,0.));
#7645=DIRECTION('ref_axis',(0.987688340595138,0.,0.156434465040231));
#7646=DIRECTION('center_axis',(0.,1.,0.));
#7647=DIRECTION('ref_axis',(1.,0.,0.));
#7648=DIRECTION('center_axis',(0.,-1.,0.));
#7649=DIRECTION('ref_axis',(1.,0.,0.));
#7650=DIRECTION('center_axis',(0.,1.,0.));
#7651=DIRECTION('ref_axis',(1.,0.,0.));
#7652=DIRECTION('center_axis',(0.,-1.,0.));
#7653=DIRECTION('ref_axis',(0.987688340595138,0.,-0.156434465040231));
#7654=DIRECTION('center_axis',(0.,1.,0.));
#7655=DIRECTION('ref_axis',(1.,0.,0.));
#7656=DIRECTION('center_axis',(0.,-1.,0.));
#7657=DIRECTION('ref_axis',(0.951056516295154,0.,-0.309016994374947));
#7658=DIRECTION('center_axis',(0.,1.,0.));
#7659=DIRECTION('ref_axis',(1.,0.,0.));
#7660=DIRECTION('center_axis',(0.,-1.,0.));
#7661=DIRECTION('ref_axis',(0.891006524188368,0.,-0.453990499739547));
#7662=DIRECTION('center_axis',(0.,1.,0.));
#7663=DIRECTION('ref_axis',(1.,0.,0.));
#7664=DIRECTION('center_axis',(0.,-1.,0.));
#7665=DIRECTION('ref_axis',(0.809016994374947,0.,-0.587785252292473));
#7666=DIRECTION('center_axis',(0.,1.,0.));
#7667=DIRECTION('ref_axis',(1.,0.,0.));
#7668=DIRECTION('center_axis',(0.,-1.,0.));
#7669=DIRECTION('ref_axis',(0.707106781186548,0.,-0.707106781186547));
#7670=DIRECTION('center_axis',(0.,1.,0.));
#7671=DIRECTION('ref_axis',(1.,0.,0.));
#7672=DIRECTION('center_axis',(0.,-1.,0.));
#7673=DIRECTION('ref_axis',(0.587785252292473,0.,-0.809016994374947));
#7674=DIRECTION('center_axis',(0.,1.,0.));
#7675=DIRECTION('ref_axis',(1.,0.,0.));
#7676=DIRECTION('center_axis',(0.,-1.,0.));
#7677=DIRECTION('ref_axis',(0.453990499739547,0.,-0.891006524188368));
#7678=DIRECTION('center_axis',(0.,1.,0.));
#7679=DIRECTION('ref_axis',(1.,0.,0.));
#7680=DIRECTION('center_axis',(0.,-1.,0.));
#7681=DIRECTION('ref_axis',(0.309016994374948,0.,-0.951056516295154));
#7682=DIRECTION('center_axis',(0.,1.,0.));
#7683=DIRECTION('ref_axis',(1.,0.,0.));
#7684=DIRECTION('center_axis',(0.,-1.,0.));
#7685=DIRECTION('ref_axis',(0.156434465040231,0.,-0.987688340595138));
#7686=DIRECTION('center_axis',(0.,1.,0.));
#7687=DIRECTION('ref_axis',(1.,0.,0.));
#7688=DIRECTION('center_axis',(0.,-1.,0.));
#7689=DIRECTION('ref_axis',(6.12323399573677E-17,0.,-1.));
#7690=DIRECTION('center_axis',(0.,1.,0.));
#7691=DIRECTION('ref_axis',(1.,0.,0.));
#7692=DIRECTION('center_axis',(0.,-1.,0.));
#7693=DIRECTION('ref_axis',(-0.156434465040231,0.,-0.987688340595138));
#7694=DIRECTION('center_axis',(0.,1.,0.));
#7695=DIRECTION('ref_axis',(1.,0.,0.));
#7696=DIRECTION('center_axis',(0.,-1.,0.));
#7697=DIRECTION('ref_axis',(-0.309016994374947,0.,-0.951056516295154));
#7698=DIRECTION('center_axis',(0.,1.,0.));
#7699=DIRECTION('ref_axis',(1.,0.,0.));
#7700=DIRECTION('center_axis',(0.,-1.,0.));
#7701=DIRECTION('ref_axis',(-0.453990499739547,0.,-0.891006524188368));
#7702=DIRECTION('center_axis',(0.,1.,0.));
#7703=DIRECTION('ref_axis',(1.,0.,0.));
#7704=DIRECTION('center_axis',(0.,-1.,0.));
#7705=DIRECTION('ref_axis',(-0.587785252292473,0.,-0.809016994374947));
#7706=DIRECTION('center_axis',(0.,1.,0.));
#7707=DIRECTION('ref_axis',(1.,0.,0.));
#7708=DIRECTION('center_axis',(0.,-1.,0.));
#7709=DIRECTION('ref_axis',(-0.707106781186547,0.,-0.707106781186548));
#7710=DIRECTION('center_axis',(0.,1.,0.));
#7711=DIRECTION('ref_axis',(1.,0.,0.));
#7712=DIRECTION('center_axis',(0.,-1.,0.));
#7713=DIRECTION('ref_axis',(-0.809016994374947,0.,-0.587785252292473));
#7714=DIRECTION('center_axis',(0.,1.,0.));
#7715=DIRECTION('ref_axis',(1.,0.,0.));
#7716=DIRECTION('center_axis',(0.,-1.,0.));
#7717=DIRECTION('ref_axis',(-0.891006524188368,0.,-0.453990499739547));
#7718=DIRECTION('center_axis',(0.,1.,0.));
#7719=DIRECTION('ref_axis',(1.,0.,0.));
#7720=DIRECTION('center_axis',(0.,-1.,0.));
#7721=DIRECTION('ref_axis',(-0.951056516295154,0.,-0.309016994374948));
#7722=DIRECTION('center_axis',(0.,1.,0.));
#7723=DIRECTION('ref_axis',(1.,0.,0.));
#7724=DIRECTION('center_axis',(0.,-1.,0.));
#7725=DIRECTION('ref_axis',(-0.987688340595138,0.,-0.156434465040231));
#7726=DIRECTION('center_axis',(0.,1.,0.));
#7727=DIRECTION('ref_axis',(1.,0.,0.));
#7728=DIRECTION('center_axis',(0.,-1.,0.));
#7729=DIRECTION('ref_axis',(-1.,0.,-1.22464679914735E-16));
#7730=DIRECTION('center_axis',(0.,1.,0.));
#7731=DIRECTION('ref_axis',(1.,0.,0.));
#7732=DIRECTION('center_axis',(0.,-1.,0.));
#7733=DIRECTION('ref_axis',(-0.987688340595138,0.,0.156434465040231));
#7734=DIRECTION('center_axis',(0.,1.,0.));
#7735=DIRECTION('ref_axis',(1.,0.,0.));
#7736=DIRECTION('center_axis',(0.,-1.,0.));
#7737=DIRECTION('ref_axis',(-0.951056516295154,0.,0.309016994374947));
#7738=DIRECTION('center_axis',(0.,1.,0.));
#7739=DIRECTION('ref_axis',(1.,0.,0.));
#7740=DIRECTION('center_axis',(0.,-1.,0.));
#7741=DIRECTION('ref_axis',(-0.891006524188368,0.,0.453990499739547));
#7742=DIRECTION('center_axis',(0.,1.,0.));
#7743=DIRECTION('ref_axis',(1.,0.,0.));
#7744=DIRECTION('center_axis',(0.,-1.,0.));
#7745=DIRECTION('ref_axis',(-0.809016994374947,0.,0.587785252292473));
#7746=DIRECTION('center_axis',(0.,1.,0.));
#7747=DIRECTION('ref_axis',(1.,0.,0.));
#7748=DIRECTION('center_axis',(0.,-1.,0.));
#7749=DIRECTION('ref_axis',(-0.707106781186548,0.,0.707106781186547));
#7750=DIRECTION('center_axis',(0.,1.,0.));
#7751=DIRECTION('ref_axis',(1.,0.,0.));
#7752=DIRECTION('center_axis',(0.,-1.,0.));
#7753=DIRECTION('ref_axis',(-0.587785252292473,0.,0.809016994374947));
#7754=DIRECTION('center_axis',(0.,1.,0.));
#7755=DIRECTION('ref_axis',(1.,0.,0.));
#7756=DIRECTION('center_axis',(0.,-1.,0.));
#7757=DIRECTION('ref_axis',(-0.453990499739547,0.,0.891006524188368));
#7758=DIRECTION('center_axis',(0.,1.,0.));
#7759=DIRECTION('ref_axis',(1.,0.,0.));
#7760=DIRECTION('center_axis',(0.,-1.,0.));
#7761=DIRECTION('ref_axis',(-0.309016994374948,0.,0.951056516295154));
#7762=DIRECTION('center_axis',(0.,1.,0.));
#7763=DIRECTION('ref_axis',(1.,0.,0.));
#7764=DIRECTION('center_axis',(0.,-1.,0.));
#7765=DIRECTION('ref_axis',(-0.156434465040231,0.,0.987688340595138));
#7766=DIRECTION('center_axis',(0.,1.,0.));
#7767=DIRECTION('ref_axis',(1.,0.,0.));
#7768=DIRECTION('center_axis',(0.,-1.,0.));
#7769=DIRECTION('ref_axis',(-1.83697019872103E-16,0.,1.));
#7770=DIRECTION('center_axis',(0.,1.,0.));
#7771=DIRECTION('ref_axis',(1.,0.,0.));
#7772=DIRECTION('center_axis',(0.,-1.,0.));
#7773=DIRECTION('ref_axis',(0.156434465040231,0.,0.987688340595138));
#7774=DIRECTION('center_axis',(0.,1.,0.));
#7775=DIRECTION('ref_axis',(1.,0.,0.));
#7776=DIRECTION('center_axis',(0.,-1.,0.));
#7777=DIRECTION('ref_axis',(0.309016994374947,0.,0.951056516295154));
#7778=DIRECTION('center_axis',(0.,1.,0.));
#7779=DIRECTION('ref_axis',(1.,0.,0.));
#7780=DIRECTION('center_axis',(0.,-1.,0.));
#7781=DIRECTION('ref_axis',(0.453990499739547,0.,0.891006524188368));
#7782=DIRECTION('center_axis',(0.,1.,0.));
#7783=DIRECTION('ref_axis',(1.,0.,0.));
#7784=DIRECTION('center_axis',(0.,-1.,0.));
#7785=DIRECTION('ref_axis',(0.587785252292473,0.,0.809016994374948));
#7786=DIRECTION('center_axis',(0.,1.,0.));
#7787=DIRECTION('ref_axis',(1.,0.,0.));
#7788=DIRECTION('center_axis',(0.,-1.,0.));
#7789=DIRECTION('ref_axis',(0.707106781186547,0.,0.707106781186548));
#7790=DIRECTION('center_axis',(0.,1.,0.));
#7791=DIRECTION('ref_axis',(1.,0.,0.));
#7792=DIRECTION('center_axis',(0.,-1.,0.));
#7793=DIRECTION('ref_axis',(0.809016994374947,0.,0.587785252292473));
#7794=DIRECTION('center_axis',(0.,1.,0.));
#7795=DIRECTION('ref_axis',(1.,0.,0.));
#7796=DIRECTION('center_axis',(0.,-1.,0.));
#7797=DIRECTION('ref_axis',(0.891006524188368,0.,0.453990499739547));
#7798=DIRECTION('center_axis',(0.,1.,0.));
#7799=DIRECTION('ref_axis',(1.,0.,0.));
#7800=DIRECTION('center_axis',(0.,-1.,0.));
#7801=DIRECTION('ref_axis',(0.951056516295154,0.,0.309016994374948));
#7802=DIRECTION('center_axis',(0.,1.,0.));
#7803=DIRECTION('ref_axis',(1.,0.,0.));
#7804=DIRECTION('center_axis',(0.,1.,0.));
#7805=DIRECTION('ref_axis',(1.,0.,0.));
#7806=DIRECTION('',(0.,-1.,0.));
#7807=DIRECTION('center_axis',(0.,1.,0.));
#7808=DIRECTION('ref_axis',(-0.987688340595137,0.,-0.156434465040233));
#7809=DIRECTION('',(0.,-1.,0.));
#7810=DIRECTION('',(0.,1.,0.));
#7811=DIRECTION('center_axis',(0.,1.,0.));
#7812=DIRECTION('ref_axis',(1.,0.,0.));
#7813=DIRECTION('',(0.,-1.,0.));
#7814=DIRECTION('center_axis',(0.,1.,0.));
#7815=DIRECTION('ref_axis',(-0.951056516295153,0.,-0.309016994374949));
#7816=DIRECTION('',(0.,1.,0.));
#7817=DIRECTION('center_axis',(0.,1.,0.));
#7818=DIRECTION('ref_axis',(1.,0.,0.));
#7819=DIRECTION('',(0.,-1.,0.));
#7820=DIRECTION('center_axis',(0.,1.,0.));
#7821=DIRECTION('ref_axis',(-0.891006524188368,0.,-0.453990499739547));
#7822=DIRECTION('',(0.,1.,0.));
#7823=DIRECTION('center_axis',(0.,1.,0.));
#7824=DIRECTION('ref_axis',(1.,0.,0.));
#7825=DIRECTION('',(0.,-1.,0.));
#7826=DIRECTION('center_axis',(0.,1.,0.));
#7827=DIRECTION('ref_axis',(-0.809016994374948,0.,-0.587785252292473));
#7828=DIRECTION('',(0.,1.,0.));
#7829=DIRECTION('center_axis',(0.,1.,0.));
#7830=DIRECTION('ref_axis',(1.,0.,0.));
#7831=DIRECTION('',(0.,-1.,0.));
#7832=DIRECTION('center_axis',(0.,1.,0.));
#7833=DIRECTION('ref_axis',(-0.707106781186547,0.,-0.707106781186548));
#7834=DIRECTION('',(0.,1.,0.));
#7835=DIRECTION('center_axis',(0.,1.,0.));
#7836=DIRECTION('ref_axis',(1.,0.,0.));
#7837=DIRECTION('',(0.,-1.,0.));
#7838=DIRECTION('center_axis',(0.,1.,0.));
#7839=DIRECTION('ref_axis',(-0.587785252292474,0.,-0.809016994374947));
#7840=DIRECTION('',(0.,1.,0.));
#7841=DIRECTION('center_axis',(0.,1.,0.));
#7842=DIRECTION('ref_axis',(1.,0.,0.));
#7843=DIRECTION('',(0.,-1.,0.));
#7844=DIRECTION('center_axis',(0.,1.,0.));
#7845=DIRECTION('ref_axis',(-0.453990499739547,0.,-0.891006524188368));
#7846=DIRECTION('',(0.,1.,0.));
#7847=DIRECTION('center_axis',(0.,1.,0.));
#7848=DIRECTION('ref_axis',(1.,0.,0.));
#7849=DIRECTION('',(0.,-1.,0.));
#7850=DIRECTION('center_axis',(0.,1.,0.));
#7851=DIRECTION('ref_axis',(-0.309016994374948,0.,-0.951056516295153));
#7852=DIRECTION('',(0.,1.,0.));
#7853=DIRECTION('center_axis',(0.,1.,0.));
#7854=DIRECTION('ref_axis',(1.,0.,0.));
#7855=DIRECTION('',(0.,-1.,0.));
#7856=DIRECTION('center_axis',(0.,1.,0.));
#7857=DIRECTION('ref_axis',(-0.156434465040232,0.,-0.987688340595138));
#7858=DIRECTION('',(0.,1.,0.));
#7859=DIRECTION('center_axis',(0.,1.,0.));
#7860=DIRECTION('ref_axis',(1.,0.,0.));
#7861=DIRECTION('',(0.,-1.,0.));
#7862=DIRECTION('center_axis',(0.,1.,0.));
#7863=DIRECTION('ref_axis',(3.06161699786838E-16,0.,-1.));
#7864=DIRECTION('',(0.,1.,0.));
#7865=DIRECTION('center_axis',(0.,1.,0.));
#7866=DIRECTION('ref_axis',(1.,0.,0.));
#7867=DIRECTION('',(0.,-1.,0.));
#7868=DIRECTION('center_axis',(0.,1.,0.));
#7869=DIRECTION('ref_axis',(0.156434465040233,0.,-0.987688340595138));
#7870=DIRECTION('',(0.,1.,0.));
#7871=DIRECTION('center_axis',(0.,1.,0.));
#7872=DIRECTION('ref_axis',(1.,0.,0.));
#7873=DIRECTION('',(0.,-1.,0.));
#7874=DIRECTION('center_axis',(0.,1.,0.));
#7875=DIRECTION('ref_axis',(0.309016994374946,0.,-0.951056516295154));
#7876=DIRECTION('',(0.,1.,0.));
#7877=DIRECTION('center_axis',(0.,1.,0.));
#7878=DIRECTION('ref_axis',(1.,0.,0.));
#7879=DIRECTION('',(0.,-1.,0.));
#7880=DIRECTION('center_axis',(0.,1.,0.));
#7881=DIRECTION('ref_axis',(0.453990499739547,0.,-0.891006524188368));
#7882=DIRECTION('',(0.,1.,0.));
#7883=DIRECTION('center_axis',(0.,1.,0.));
#7884=DIRECTION('ref_axis',(1.,0.,0.));
#7885=DIRECTION('',(0.,-1.,0.));
#7886=DIRECTION('center_axis',(0.,1.,0.));
#7887=DIRECTION('ref_axis',(0.587785252292473,0.,-0.809016994374947));
#7888=DIRECTION('',(0.,1.,0.));
#7889=DIRECTION('center_axis',(0.,1.,0.));
#7890=DIRECTION('ref_axis',(1.,0.,0.));
#7891=DIRECTION('',(0.,-1.,0.));
#7892=DIRECTION('center_axis',(0.,1.,0.));
#7893=DIRECTION('ref_axis',(0.707106781186548,0.,-0.707106781186547));
#7894=DIRECTION('',(0.,1.,0.));
#7895=DIRECTION('center_axis',(0.,1.,0.));
#7896=DIRECTION('ref_axis',(1.,0.,0.));
#7897=DIRECTION('',(0.,-1.,0.));
#7898=DIRECTION('center_axis',(0.,1.,0.));
#7899=DIRECTION('ref_axis',(0.809016994374946,0.,-0.587785252292475));
#7900=DIRECTION('',(0.,1.,0.));
#7901=DIRECTION('center_axis',(0.,1.,0.));
#7902=DIRECTION('ref_axis',(1.,0.,0.));
#7903=DIRECTION('',(0.,-1.,0.));
#7904=DIRECTION('center_axis',(0.,1.,0.));
#7905=DIRECTION('ref_axis',(0.891006524188368,0.,-0.453990499739547));
#7906=DIRECTION('',(0.,1.,0.));
#7907=DIRECTION('center_axis',(0.,1.,0.));
#7908=DIRECTION('ref_axis',(1.,0.,0.));
#7909=DIRECTION('',(0.,-1.,0.));
#7910=DIRECTION('center_axis',(0.,1.,0.));
#7911=DIRECTION('ref_axis',(0.951056516295154,0.,-0.309016994374946));
#7912=DIRECTION('',(0.,1.,0.));
#7913=DIRECTION('center_axis',(0.,1.,0.));
#7914=DIRECTION('ref_axis',(1.,0.,0.));
#7915=DIRECTION('',(0.,-1.,0.));
#7916=DIRECTION('center_axis',(0.,1.,0.));
#7917=DIRECTION('ref_axis',(0.987688340595138,0.,-0.156434465040232));
#7918=DIRECTION('',(0.,1.,0.));
#7919=DIRECTION('center_axis',(0.,1.,0.));
#7920=DIRECTION('ref_axis',(1.,0.,0.));
#7921=DIRECTION('',(0.,-1.,0.));
#7922=DIRECTION('center_axis',(0.,1.,0.));
#7923=DIRECTION('ref_axis',(1.,0.,2.44929359829471E-16));
#7924=DIRECTION('',(0.,1.,0.));
#7925=DIRECTION('center_axis',(0.,1.,0.));
#7926=DIRECTION('ref_axis',(1.,0.,0.));
#7927=DIRECTION('',(0.,-1.,0.));
#7928=DIRECTION('center_axis',(0.,1.,0.));
#7929=DIRECTION('ref_axis',(0.987688340595137,0.,0.156434465040232));
#7930=DIRECTION('',(0.,1.,0.));
#7931=DIRECTION('center_axis',(0.,1.,0.));
#7932=DIRECTION('ref_axis',(1.,0.,0.));
#7933=DIRECTION('',(0.,-1.,0.));
#7934=DIRECTION('center_axis',(0.,1.,0.));
#7935=DIRECTION('ref_axis',(0.951056516295154,0.,0.309016994374946));
#7936=DIRECTION('',(0.,1.,0.));
#7937=DIRECTION('center_axis',(0.,1.,0.));
#7938=DIRECTION('ref_axis',(1.,0.,0.));
#7939=DIRECTION('',(0.,-1.,0.));
#7940=DIRECTION('center_axis',(0.,1.,0.));
#7941=DIRECTION('ref_axis',(0.891006524188368,0.,0.453990499739547));
#7942=DIRECTION('',(0.,1.,0.));
#7943=DIRECTION('center_axis',(0.,1.,0.));
#7944=DIRECTION('ref_axis',(1.,0.,0.));
#7945=DIRECTION('',(0.,-1.,0.));
#7946=DIRECTION('center_axis',(0.,1.,0.));
#7947=DIRECTION('ref_axis',(0.809016994374947,0.,0.587785252292473));
#7948=DIRECTION('',(0.,1.,0.));
#7949=DIRECTION('center_axis',(0.,1.,0.));
#7950=DIRECTION('ref_axis',(1.,0.,0.));
#7951=DIRECTION('',(0.,-1.,0.));
#7952=DIRECTION('center_axis',(0.,1.,0.));
#7953=DIRECTION('ref_axis',(0.707106781186547,0.,0.707106781186548));
#7954=DIRECTION('',(0.,1.,0.));
#7955=DIRECTION('center_axis',(0.,1.,0.));
#7956=DIRECTION('ref_axis',(1.,0.,0.));
#7957=DIRECTION('',(0.,-1.,0.));
#7958=DIRECTION('center_axis',(0.,1.,0.));
#7959=DIRECTION('ref_axis',(0.587785252292475,0.,0.809016994374946));
#7960=DIRECTION('',(0.,1.,0.));
#7961=DIRECTION('center_axis',(0.,1.,0.));
#7962=DIRECTION('ref_axis',(1.,0.,0.));
#7963=DIRECTION('',(0.,-1.,0.));
#7964=DIRECTION('center_axis',(0.,1.,0.));
#7965=DIRECTION('ref_axis',(0.453990499739547,0.,0.891006524188368));
#7966=DIRECTION('',(0.,1.,0.));
#7967=DIRECTION('center_axis',(0.,1.,0.));
#7968=DIRECTION('ref_axis',(1.,0.,0.));
#7969=DIRECTION('',(0.,-1.,0.));
#7970=DIRECTION('center_axis',(0.,1.,0.));
#7971=DIRECTION('ref_axis',(0.309016994374946,0.,0.951056516295154));
#7972=DIRECTION('',(0.,1.,0.));
#7973=DIRECTION('center_axis',(0.,1.,0.));
#7974=DIRECTION('ref_axis',(1.,0.,0.));
#7975=DIRECTION('',(0.,-1.,0.));
#7976=DIRECTION('center_axis',(0.,1.,0.));
#7977=DIRECTION('ref_axis',(0.156434465040232,0.,0.987688340595138));
#7978=DIRECTION('',(0.,1.,0.));
#7979=DIRECTION('center_axis',(0.,1.,0.));
#7980=DIRECTION('ref_axis',(1.,0.,0.));
#7981=DIRECTION('',(0.,-1.,0.));
#7982=DIRECTION('center_axis',(0.,1.,0.));
#7983=DIRECTION('ref_axis',(-1.83697019872103E-16,0.,1.));
#7984=DIRECTION('',(0.,1.,0.));
#7985=DIRECTION('center_axis',(0.,1.,0.));
#7986=DIRECTION('ref_axis',(1.,0.,0.));
#7987=DIRECTION('',(0.,-1.,0.));
#7988=DIRECTION('center_axis',(0.,1.,0.));
#7989=DIRECTION('ref_axis',(-0.156434465040232,0.,0.987688340595138));
#7990=DIRECTION('',(0.,1.,0.));
#7991=DIRECTION('center_axis',(0.,1.,0.));
#7992=DIRECTION('ref_axis',(1.,0.,0.));
#7993=DIRECTION('',(0.,-1.,0.));
#7994=DIRECTION('center_axis',(0.,1.,0.));
#7995=DIRECTION('ref_axis',(-0.309016994374946,0.,0.951056516295154));
#7996=DIRECTION('',(0.,1.,0.));
#7997=DIRECTION('center_axis',(0.,1.,0.));
#7998=DIRECTION('ref_axis',(1.,0.,0.));
#7999=DIRECTION('',(0.,-1.,0.));
#8000=DIRECTION('center_axis',(0.,1.,0.));
#8001=DIRECTION('ref_axis',(-0.453990499739549,0.,0.891006524188367));
#8002=DIRECTION('',(0.,1.,0.));
#8003=DIRECTION('center_axis',(0.,1.,0.));
#8004=DIRECTION('ref_axis',(1.,0.,0.));
#8005=DIRECTION('',(0.,-1.,0.));
#8006=DIRECTION('center_axis',(0.,1.,0.));
#8007=DIRECTION('ref_axis',(-0.587785252292474,0.,0.809016994374947));
#8008=DIRECTION('',(0.,1.,0.));
#8009=DIRECTION('center_axis',(0.,1.,0.));
#8010=DIRECTION('ref_axis',(1.,0.,0.));
#8011=DIRECTION('',(0.,-1.,0.));
#8012=DIRECTION('center_axis',(0.,1.,0.));
#8013=DIRECTION('ref_axis',(-0.707106781186548,0.,0.707106781186547));
#8014=DIRECTION('',(0.,1.,0.));
#8015=DIRECTION('center_axis',(0.,1.,0.));
#8016=DIRECTION('ref_axis',(1.,0.,0.));
#8017=DIRECTION('',(0.,-1.,0.));
#8018=DIRECTION('center_axis',(0.,1.,0.));
#8019=DIRECTION('ref_axis',(-0.809016994374947,0.,0.587785252292474));
#8020=DIRECTION('',(0.,1.,0.));
#8021=DIRECTION('center_axis',(0.,1.,0.));
#8022=DIRECTION('ref_axis',(1.,0.,0.));
#8023=DIRECTION('',(0.,-1.,0.));
#8024=DIRECTION('center_axis',(0.,1.,0.));
#8025=DIRECTION('ref_axis',(-0.891006524188368,0.,0.453990499739547));
#8026=DIRECTION('',(0.,1.,0.));
#8027=DIRECTION('center_axis',(0.,1.,0.));
#8028=DIRECTION('ref_axis',(1.,0.,0.));
#8029=DIRECTION('',(0.,-1.,0.));
#8030=DIRECTION('center_axis',(0.,1.,0.));
#8031=DIRECTION('ref_axis',(-0.951056516295154,0.,0.309016994374948));
#8032=DIRECTION('',(0.,1.,0.));
#8033=DIRECTION('center_axis',(0.,1.,0.));
#8034=DIRECTION('ref_axis',(1.,0.,0.));
#8035=DIRECTION('',(0.,-1.,0.));
#8036=DIRECTION('center_axis',(0.,1.,0.));
#8037=DIRECTION('ref_axis',(-0.987688340595137,0.,0.156434465040233));
#8038=DIRECTION('',(0.,1.,0.));
#8039=DIRECTION('center_axis',(0.,1.,0.));
#8040=DIRECTION('ref_axis',(1.,0.,0.));
#8041=DIRECTION('',(0.,1.,0.));
#8042=DIRECTION('center_axis',(0.,1.,0.));
#8043=DIRECTION('ref_axis',(-1.,0.,-1.22464679914735E-16));
#8044=DIRECTION('',(0.,-1.,0.));
#8045=DIRECTION('center_axis',(0.,1.,0.));
#8046=DIRECTION('ref_axis',(1.,0.,0.));
#8047=DIRECTION('axis',(0.,0.,1.));
#8048=DIRECTION('refdir',(1.,0.,0.));
#8049=DIRECTION('center_axis',(1.,0.,0.));
#8050=DIRECTION('ref_axis',(0.,0.,-1.));
#8051=DIRECTION('',(0.,0.707106781186547,-0.707106781186548));
#8052=DIRECTION('',(0.,1.,0.));
#8053=DIRECTION('',(0.,0.707106781186547,0.707106781186548));
#8054=DIRECTION('',(0.,0.,1.));
#8055=DIRECTION('',(0.,-0.707106781186548,0.707106781186548));
#8056=DIRECTION('',(0.,-1.,0.));
#8057=DIRECTION('',(0.,-0.707106781186548,-0.707106781186548));
#8058=DIRECTION('',(0.,0.,-1.));
#8059=DIRECTION('center_axis',(0.,-0.707106781186548,-0.707106781186548));
#8060=DIRECTION('ref_axis',(-1.,0.,0.));
#8061=DIRECTION('',(-1.,0.,0.));
#8062=DIRECTION('',(0.,0.707106781186548,-0.707106781186548));
#8063=DIRECTION('',(1.,0.,0.));
#8064=DIRECTION('center_axis',(0.,-1.,0.));
#8065=DIRECTION('ref_axis',(1.,0.,0.));
#8066=DIRECTION('',(1.,0.,0.));
#8067=DIRECTION('',(0.,0.,-1.));
#8068=DIRECTION('center_axis',(0.,-0.707106781186548,0.707106781186547));
#8069=DIRECTION('ref_axis',(1.,0.,0.));
#8070=DIRECTION('',(-1.,0.,0.));
#8071=DIRECTION('',(0.,-0.707106781186547,-0.707106781186548));
#8072=DIRECTION('center_axis',(0.,0.,1.));
#8073=DIRECTION('ref_axis',(1.,0.,0.));
#8074=DIRECTION('',(1.,0.,0.));
#8075=DIRECTION('',(0.,-1.,0.));
#8076=DIRECTION('center_axis',(1.,0.,0.));
#8077=DIRECTION('ref_axis',(0.,0.,-1.));
#8078=DIRECTION('',(0.,-0.707106781186547,0.707106781186548));
#8079=DIRECTION('',(0.,0.,1.));
#8080=DIRECTION('',(0.,0.707106781186548,0.707106781186548));
#8081=DIRECTION('',(0.,1.,0.));
#8082=DIRECTION('center_axis',(0.,0.707106781186548,0.707106781186547));
#8083=DIRECTION('ref_axis',(1.,0.,0.));
#8084=DIRECTION('',(-1.,0.,0.));
#8085=DIRECTION('center_axis',(0.,1.,0.));
#8086=DIRECTION('ref_axis',(-1.,0.,0.));
#8087=DIRECTION('',(1.,0.,0.));
#8088=DIRECTION('center_axis',(0.,0.707106781186548,-0.707106781186548));
#8089=DIRECTION('ref_axis',(-1.,0.,0.));
#8090=DIRECTION('',(-1.,0.,0.));
#8091=DIRECTION('center_axis',(0.,0.,1.));
#8092=DIRECTION('ref_axis',(1.,0.,0.));
#8093=DIRECTION('axis',(0.,0.,1.));
#8094=DIRECTION('refdir',(1.,0.,0.));
#8095=DIRECTION('center_axis',(0.,1.,0.));
#8096=DIRECTION('ref_axis',(0.,0.,1.));
#8097=DIRECTION('center_axis',(0.,-1.,0.));
#8098=DIRECTION('ref_axis',(1.,0.,0.));
#8099=DIRECTION('center_axis',(0.,-1.,0.));
#8100=DIRECTION('ref_axis',(1.,0.,0.));
#8101=DIRECTION('center_axis',(0.,-1.,0.));
#8102=DIRECTION('ref_axis',(1.,0.,0.));
#8103=DIRECTION('',(0.707106781186548,0.707106781186547,8.65956056235493E-17));
#8104=DIRECTION('center_axis',(0.,-1.,0.));
#8105=DIRECTION('ref_axis',(1.,0.,0.));
#8106=DIRECTION('center_axis',(0.,-1.,0.));
#8107=DIRECTION('ref_axis',(1.,0.,0.));
#8108=DIRECTION('',(0.,1.,0.));
#8109=DIRECTION('center_axis',(0.,1.,0.));
#8110=DIRECTION('ref_axis',(1.,0.,0.));
#8111=DIRECTION('center_axis',(0.,-1.,0.));
#8112=DIRECTION('ref_axis',(1.,0.,0.));
#8113=DIRECTION('',(-0.707106781186547,0.707106781186548,-8.65956056235493E-17));
#8114=DIRECTION('center_axis',(0.,-1.,0.));
#8115=DIRECTION('ref_axis',(0.,0.,-1.));
#8116=DIRECTION('center_axis',(0.,-1.,0.));
#8117=DIRECTION('ref_axis',(1.,0.,0.));
#8118=DIRECTION('center_axis',(0.,1.,0.));
#8119=DIRECTION('ref_axis',(1.,0.,0.));
#8120=DIRECTION('center_axis',(0.,1.,0.));
#8121=DIRECTION('ref_axis',(1.,0.,0.));
#8122=DIRECTION('',(-0.447213595499958,0.894427190999916,-5.47678698264203E-17));
#8123=DIRECTION('center_axis',(0.,-1.,0.));
#8124=DIRECTION('ref_axis',(1.,0.,0.));
#8125=DIRECTION('center_axis',(0.,1.,0.));
#8126=DIRECTION('ref_axis',(1.,0.,0.));
#8127=DIRECTION('',(0.,1.,0.));
#8128=DIRECTION('center_axis',(0.,1.,0.));
#8129=DIRECTION('ref_axis',(1.,0.,0.));
#8130=DIRECTION('center_axis',(0.,-1.,0.));
#8131=DIRECTION('ref_axis',(1.,0.,0.));
#8132=DIRECTION('',(-0.707106781186547,0.707106781186548,-8.65956056235493E-17));
#8133=DIRECTION('center_axis',(0.,-1.,0.));
#8134=DIRECTION('ref_axis',(0.,0.,-1.));
#8135=DIRECTION('center_axis',(0.866025403784439,0.,-0.5));
#8136=DIRECTION('ref_axis',(0.5,0.,0.866025403784439));
#8137=DIRECTION('',(-0.5,0.,-0.866025403784439));
#8138=DIRECTION('',(0.,-1.,0.));
#8139=DIRECTION('',(0.5,0.,0.866025403784439));
#8140=DIRECTION('',(0.,-1.,0.));
#8141=DIRECTION('center_axis',(1.20185167898973E-16,0.,-1.));
#8142=DIRECTION('ref_axis',(1.,0.,1.20185167898973E-16));
#8143=DIRECTION('',(-1.,0.,-1.20185167898973E-16));
#8144=DIRECTION('',(0.,-1.,0.));
#8145=DIRECTION('',(1.,0.,1.20185167898973E-16));
#8146=DIRECTION('center_axis',(-0.866025403784439,0.,-0.5));
#8147=DIRECTION('ref_axis',(0.5,0.,-0.866025403784439));
#8148=DIRECTION('',(-0.5,0.,0.866025403784439));
#8149=DIRECTION('',(0.,-1.,0.));
#8150=DIRECTION('',(0.5,0.,-0.866025403784439));
#8151=DIRECTION('center_axis',(-0.866025403784439,0.,0.5));
#8152=DIRECTION('ref_axis',(-0.5,0.,-0.866025403784439));
#8153=DIRECTION('',(0.5,0.,0.866025403784439));
#8154=DIRECTION('',(0.,-1.,0.));
#8155=DIRECTION('',(-0.5,0.,-0.866025403784439));
#8156=DIRECTION('center_axis',(-2.40370335797945E-16,0.,1.));
#8157=DIRECTION('ref_axis',(-1.,0.,-2.40370335797945E-16));
#8158=DIRECTION('',(1.,0.,2.40370335797945E-16));
#8159=DIRECTION('',(0.,-1.,0.));
#8160=DIRECTION('',(-1.,0.,-2.40370335797945E-16));
#8161=DIRECTION('center_axis',(0.866025403784439,0.,0.5));
#8162=DIRECTION('ref_axis',(-0.5,0.,0.866025403784439));
#8163=DIRECTION('',(0.5,0.,-0.866025403784439));
#8164=DIRECTION('',(-0.5,0.,0.866025403784439));
#8165=DIRECTION('center_axis',(0.,1.,0.));
#8166=DIRECTION('ref_axis',(1.,0.,0.));
#8167=DIRECTION('center_axis',(0.,-1.,0.));
#8168=DIRECTION('ref_axis',(0.,0.,-1.));
#8169=DIRECTION('axis',(0.,0.,1.));
#8170=DIRECTION('refdir',(1.,0.,0.));
#8171=DIRECTION('center_axis',(1.,0.,0.));
#8172=DIRECTION('ref_axis',(0.,0.,-1.));
#8173=DIRECTION('',(0.,-0.707106781186547,-0.707106781186548));
#8174=DIRECTION('',(0.,-1.,0.));
#8175=DIRECTION('',(0.,-0.707106781186547,0.707106781186548));
#8176=DIRECTION('',(0.,0.,1.));
#8177=DIRECTION('',(0.,0.707106781186547,0.707106781186548));
#8178=DIRECTION('',(0.,1.,0.));
#8179=DIRECTION('',(0.,0.707106781186547,-0.707106781186548));
#8180=DIRECTION('',(0.,0.,-1.));
#8181=DIRECTION('center_axis',(0.,0.707106781186548,-0.707106781186547));
#8182=DIRECTION('ref_axis',(-1.,0.,0.));
#8183=DIRECTION('',(1.,0.,0.));
#8184=DIRECTION('',(0.,-0.707106781186547,-0.707106781186548));
#8185=DIRECTION('',(-1.,0.,0.));
#8186=DIRECTION('center_axis',(0.,1.,0.));
#8187=DIRECTION('ref_axis',(-1.,0.,0.));
#8188=DIRECTION('',(-1.,0.,0.));
#8189=DIRECTION('',(0.,0.,-1.));
#8190=DIRECTION('center_axis',(0.,0.707106781186548,0.707106781186547));
#8191=DIRECTION('ref_axis',(1.,0.,0.));
#8192=DIRECTION('',(1.,0.,0.));
#8193=DIRECTION('',(0.,0.707106781186547,-0.707106781186548));
#8194=DIRECTION('center_axis',(0.,0.,1.));
#8195=DIRECTION('ref_axis',(1.,0.,0.));
#8196=DIRECTION('',(-1.,0.,0.));
#8197=DIRECTION('',(0.,1.,0.));
#8198=DIRECTION('center_axis',(1.,0.,0.));
#8199=DIRECTION('ref_axis',(0.,0.,-1.));
#8200=DIRECTION('',(0.,-0.707106781186547,0.707106781186548));
#8201=DIRECTION('',(0.,-1.,0.));
#8202=DIRECTION('',(0.,0.707106781186547,0.707106781186548));
#8203=DIRECTION('',(0.,0.,1.));
#8204=DIRECTION('center_axis',(0.,0.,1.));
#8205=DIRECTION('ref_axis',(1.,0.,0.));
#8206=DIRECTION('',(1.,0.,0.));
#8207=DIRECTION('center_axis',(0.,-0.707106781186548,0.707106781186547));
#8208=DIRECTION('ref_axis',(1.,0.,0.));
#8209=DIRECTION('',(1.,0.,0.));
#8210=DIRECTION('center_axis',(0.,-0.707106781186548,-0.707106781186547));
#8211=DIRECTION('ref_axis',(-1.,0.,0.));
#8212=DIRECTION('',(-1.,0.,0.));
#8213=DIRECTION('center_axis',(0.,-1.,0.));
#8214=DIRECTION('ref_axis',(1.,0.,0.));
#8215=DIRECTION('axis',(0.,0.,1.));
#8216=DIRECTION('refdir',(1.,0.,0.));
#8217=DIRECTION('center_axis',(0.866025403784439,0.,-0.5));
#8218=DIRECTION('ref_axis',(0.5,0.,0.866025403784439));
#8219=DIRECTION('',(0.5,0.,0.866025403784439));
#8220=DIRECTION('',(0.,-1.,0.));
#8221=DIRECTION('',(0.5,0.,0.866025403784439));
#8222=DIRECTION('',(0.,-1.,0.));
#8223=DIRECTION('center_axis',(1.92296268638356E-16,0.,-1.));
#8224=DIRECTION('ref_axis',(1.,0.,1.92296268638356E-16));
#8225=DIRECTION('',(1.,0.,1.92296268638356E-16));
#8226=DIRECTION('',(0.,-1.,0.));
#8227=DIRECTION('',(1.,0.,1.92296268638356E-16));
#8228=DIRECTION('center_axis',(-0.866025403784439,0.,-0.5));
#8229=DIRECTION('ref_axis',(0.5,0.,-0.866025403784439));
#8230=DIRECTION('',(0.5,0.,-0.866025403784439));
#8231=DIRECTION('',(0.,-1.,0.));
#8232=DIRECTION('',(0.5,0.,-0.866025403784438));
#8233=DIRECTION('center_axis',(-0.866025403784439,0.,0.5));
#8234=DIRECTION('ref_axis',(-0.5,0.,-0.866025403784439));
#8235=DIRECTION('',(-0.5,0.,-0.866025403784439));
#8236=DIRECTION('',(0.,-1.,0.));
#8237=DIRECTION('',(-0.5,0.,-0.866025403784439));
#8238=DIRECTION('center_axis',(-1.92296268638356E-16,0.,1.));
#8239=DIRECTION('ref_axis',(-1.,0.,-1.92296268638356E-16));
#8240=DIRECTION('',(-1.,0.,-1.92296268638356E-16));
#8241=DIRECTION('',(0.,-1.,0.));
#8242=DIRECTION('',(-1.,0.,-1.92296268638356E-16));
#8243=DIRECTION('center_axis',(0.866025403784439,0.,0.5));
#8244=DIRECTION('ref_axis',(-0.5,0.,0.866025403784439));
#8245=DIRECTION('',(-0.5,0.,0.866025403784439));
#8246=DIRECTION('',(-0.5,0.,0.866025403784439));
#8247=DIRECTION('center_axis',(0.,-1.,0.));
#8248=DIRECTION('ref_axis',(0.,0.,-1.));
#8249=DIRECTION('center_axis',(0.,1.,0.));
#8250=DIRECTION('ref_axis',(0.,0.,1.));
#8251=DIRECTION('center_axis',(0.,-1.,0.));
#8252=DIRECTION('ref_axis',(1.,0.,0.));
#8253=DIRECTION('center_axis',(0.,-1.,0.));
#8254=DIRECTION('ref_axis',(1.,0.,0.));
#8255=DIRECTION('center_axis',(0.,-1.,0.));
#8256=DIRECTION('ref_axis',(1.,0.,0.));
#8257=DIRECTION('',(0.707106781186547,0.707106781186548,8.65956056235493E-17));
#8258=DIRECTION('center_axis',(0.,-1.,0.));
#8259=DIRECTION('ref_axis',(1.,0.,0.));
#8260=DIRECTION('center_axis',(0.,1.,0.));
#8261=DIRECTION('ref_axis',(1.,0.,0.));
#8262=DIRECTION('',(0.,1.,0.));
#8263=DIRECTION('center_axis',(0.,1.,0.));
#8264=DIRECTION('ref_axis',(1.,0.,0.));
#8265=DIRECTION('center_axis',(0.,-1.,0.));
#8266=DIRECTION('ref_axis',(1.,0.,0.));
#8267=DIRECTION('',(-0.707106781186547,0.707106781186548,-8.65956056235493E-17));
#8268=DIRECTION('center_axis',(0.,-1.,0.));
#8269=DIRECTION('ref_axis',(0.,0.,-1.));
#8270=DIRECTION('',(0.,0.,1.));
#8271=DIRECTION('',(1.,0.,0.));
#8272=DIRECTION('',(0.,0.,1.));
#8273=DIRECTION('',(1.,0.,0.));
#8274=DIRECTION('',(0.,0.,1.));
#8275=DIRECTION('',(1.,0.,0.));
#8276=DIRECTION('',(0.,0.,1.));
#8277=DIRECTION('',(1.,0.,0.));
#8278=DIRECTION('',(0.,0.,1.));
#8279=DIRECTION('',(1.,0.,0.));
#8280=DIRECTION('',(0.,0.,1.));
#8281=DIRECTION('',(1.,0.,0.));
#8282=DIRECTION('',(0.,0.,1.));
#8283=DIRECTION('',(1.,0.,0.));
#8284=DIRECTION('',(0.,0.,1.));
#8285=DIRECTION('',(1.,0.,0.));
#8286=DIRECTION('',(0.,0.,1.));
#8287=DIRECTION('',(1.,0.,0.));
#8288=DIRECTION('',(0.,0.,1.));
#8289=DIRECTION('',(1.,0.,0.));
#8290=DIRECTION('',(8.65956056235493E-17,-8.65956056235493E-17,-1.));
#8291=DIRECTION('',(2.22044604925031E-16,1.,-8.65956056235494E-17));
#8292=DIRECTION('',(0.,0.,1.));
#8293=DIRECTION('',(1.,0.,0.));
#8294=DIRECTION('',(8.65956056235493E-17,-8.65956056235493E-17,-1.));
#8295=DIRECTION('',(2.22044604925031E-16,1.,-8.65956056235494E-17));
#8296=DIRECTION('',(0.,0.,1.));
#8297=DIRECTION('',(-1.,1.22464679914735E-16,0.));
#8298=DIRECTION('',(0.,0.,1.));
#8299=DIRECTION('',(1.,0.,0.));
#8300=DIRECTION('',(8.65956056235493E-17,-8.65956056235493E-17,-1.));
#8301=DIRECTION('',(2.22044604925031E-16,1.,-8.65956056235494E-17));
#8302=DIRECTION('',(0.,-1.,2.22044604925031E-16));
#8303=DIRECTION('',(1.,0.,0.));
#8304=DIRECTION('',(0.,-1.,2.22044604925031E-16));
#8305=DIRECTION('',(1.,0.,0.));
#8306=DIRECTION('',(0.,-1.,2.22044604925031E-16));
#8307=DIRECTION('',(1.,0.,0.));
#8308=DIRECTION('',(0.,0.,1.));
#8309=DIRECTION('',(1.,0.,0.));
#8310=DIRECTION('',(0.,0.,1.));
#8311=DIRECTION('',(1.,0.,0.));
#8312=CARTESIAN_POINT('',(0.,0.,0.));
#8313=CARTESIAN_POINT('',(0.,0.,0.));
#8314=CARTESIAN_POINT('',(0.,0.,0.));
#8315=CARTESIAN_POINT('Origin',(4.75,0.,-0.1));
#8316=CARTESIAN_POINT('',(4.41,-4.163799117101E-17,0.));
#8317=CARTESIAN_POINT('Origin',(4.75,0.,0.));
#8318=CARTESIAN_POINT('',(4.41,4.163799117101E-17,1.2));
#8319=CARTESIAN_POINT('',(4.41,-4.163799117101E-17,-0.1));
#8320=CARTESIAN_POINT('Origin',(4.75,0.,1.2));
#8321=CARTESIAN_POINT('Origin',(-4.75,20.,-0.1));
#8322=CARTESIAN_POINT('',(-5.09,20.,0.));
#8323=CARTESIAN_POINT('Origin',(-4.75,20.,0.));
#8324=CARTESIAN_POINT('',(-5.09,20.,1.2));
#8325=CARTESIAN_POINT('',(-5.09,20.,-0.1));
#8326=CARTESIAN_POINT('Origin',(-4.75,20.,1.2));
#8327=CARTESIAN_POINT('Origin',(-4.75,0.,-0.1));
#8328=CARTESIAN_POINT('',(-5.09,-4.163799117101E-17,0.));
#8329=CARTESIAN_POINT('Origin',(-4.75,0.,0.));
#8330=CARTESIAN_POINT('',(-5.09,4.163799117101E-17,1.2));
#8331=CARTESIAN_POINT('',(-5.09,-4.163799117101E-17,-0.1));
#8332=CARTESIAN_POINT('Origin',(-4.75,0.,1.2));
#8333=CARTESIAN_POINT('Origin',(4.75,20.,-0.1));
#8334=CARTESIAN_POINT('',(4.41,20.,0.));
#8335=CARTESIAN_POINT('Origin',(4.75,20.,0.));
#8336=CARTESIAN_POINT('',(4.41,20.,1.2));
#8337=CARTESIAN_POINT('',(4.41,20.,-0.1));
#8338=CARTESIAN_POINT('Origin',(4.75,20.,1.2));
#8339=CARTESIAN_POINT('Origin',(8.,29.,0.));
#8340=CARTESIAN_POINT('',(8.,29.,0.));
#8341=CARTESIAN_POINT('',(-8.,29.,0.));
#8342=CARTESIAN_POINT('',(8.,29.,0.));
#8343=CARTESIAN_POINT('',(-8.,29.,1.2));
#8344=CARTESIAN_POINT('',(-8.,29.,0.));
#8345=CARTESIAN_POINT('',(8.,29.,1.2));
#8346=CARTESIAN_POINT('',(8.,29.,1.2));
#8347=CARTESIAN_POINT('',(8.,29.,0.));
#8348=CARTESIAN_POINT('Origin',(8.,-7.,0.));
#8349=CARTESIAN_POINT('',(8.,-7.,0.));
#8350=CARTESIAN_POINT('',(8.,-7.,0.));
#8351=CARTESIAN_POINT('',(8.,-7.,1.2));
#8352=CARTESIAN_POINT('',(8.,-7.,1.2));
#8353=CARTESIAN_POINT('',(8.,-7.,0.));
#8354=CARTESIAN_POINT('Origin',(-8.,-7.,0.));
#8355=CARTESIAN_POINT('',(-8.,-7.,0.));
#8356=CARTESIAN_POINT('',(-8.,-7.,0.));
#8357=CARTESIAN_POINT('',(-8.,-7.,1.2));
#8358=CARTESIAN_POINT('',(-8.,-7.,1.2));
#8359=CARTESIAN_POINT('',(-8.,-7.,0.));
#8360=CARTESIAN_POINT('Origin',(-8.,29.,0.));
#8361=CARTESIAN_POINT('',(-8.,29.,0.));
#8362=CARTESIAN_POINT('',(-8.,29.,1.2));
#8363=CARTESIAN_POINT('Origin',(0.,11.,1.2));
#8364=CARTESIAN_POINT('Origin',(0.,11.,0.));
#8365=CARTESIAN_POINT('',(0.,0.,0.));
#8366=CARTESIAN_POINT('Origin',(8.,-6.,-0.3));
#8367=CARTESIAN_POINT('',(8.,-6.,-0.3));
#8368=CARTESIAN_POINT('',(-8.,-6.,-0.3));
#8369=CARTESIAN_POINT('',(8.,-6.,-0.3));
#8370=CARTESIAN_POINT('',(-8.,-6.,0.));
#8371=CARTESIAN_POINT('',(-8.,-6.,-0.3));
#8372=CARTESIAN_POINT('',(8.,-6.,0.));
#8373=CARTESIAN_POINT('',(8.,-6.,0.));
#8374=CARTESIAN_POINT('',(8.,-6.,-0.3));
#8375=CARTESIAN_POINT('Origin',(8.,-7.,-0.3));
#8376=CARTESIAN_POINT('',(8.,-7.,-0.3));
#8377=CARTESIAN_POINT('',(8.,-7.,-0.3));
#8378=CARTESIAN_POINT('',(8.,-7.,0.));
#8379=CARTESIAN_POINT('',(8.,-7.,0.));
#8380=CARTESIAN_POINT('',(8.,-7.,-0.3));
#8381=CARTESIAN_POINT('Origin',(-8.,-7.,-0.3));
#8382=CARTESIAN_POINT('',(-8.,-7.,-0.3));
#8383=CARTESIAN_POINT('',(-8.,-7.,-0.3));
#8384=CARTESIAN_POINT('',(-8.,-7.,0.));
#8385=CARTESIAN_POINT('',(-8.,-7.,0.));
#8386=CARTESIAN_POINT('',(-8.,-7.,-0.3));
#8387=CARTESIAN_POINT('Origin',(-8.,-6.,-0.3));
#8388=CARTESIAN_POINT('',(-8.,-6.,-0.3));
#8389=CARTESIAN_POINT('',(-8.,-6.,0.));
#8390=CARTESIAN_POINT('Origin',(0.,-6.5,0.));
#8391=CARTESIAN_POINT('Origin',(0.,-6.5,-0.3));
#8392=CARTESIAN_POINT('',(0.,0.,0.));
#8393=CARTESIAN_POINT('Origin',(8.,29.,-0.3));
#8394=CARTESIAN_POINT('',(8.,29.,-0.3));
#8395=CARTESIAN_POINT('',(-8.,29.,-0.3));
#8396=CARTESIAN_POINT('',(8.,29.,-0.3));
#8397=CARTESIAN_POINT('',(-8.,29.,0.));
#8398=CARTESIAN_POINT('',(-8.,29.,-0.3));
#8399=CARTESIAN_POINT('',(8.,29.,0.));
#8400=CARTESIAN_POINT('',(8.,29.,0.));
#8401=CARTESIAN_POINT('',(8.,29.,-0.3));
#8402=CARTESIAN_POINT('Origin',(8.,28.,-0.3));
#8403=CARTESIAN_POINT('',(8.,28.,-0.3));
#8404=CARTESIAN_POINT('',(8.,28.,-0.3));
#8405=CARTESIAN_POINT('',(8.,28.,0.));
#8406=CARTESIAN_POINT('',(8.,28.,0.));
#8407=CARTESIAN_POINT('',(8.,28.,-0.3));
#8408=CARTESIAN_POINT('Origin',(-8.,28.,-0.3));
#8409=CARTESIAN_POINT('',(-8.,28.,-0.3));
#8410=CARTESIAN_POINT('',(-8.,28.,-0.3));
#8411=CARTESIAN_POINT('',(-8.,28.,0.));
#8412=CARTESIAN_POINT('',(-8.,28.,0.));
#8413=CARTESIAN_POINT('',(-8.,28.,-0.3));
#8414=CARTESIAN_POINT('Origin',(-8.,29.,-0.3));
#8415=CARTESIAN_POINT('',(-8.,29.,-0.3));
#8416=CARTESIAN_POINT('',(-8.,29.,0.));
#8417=CARTESIAN_POINT('Origin',(0.,28.5,0.));
#8418=CARTESIAN_POINT('Origin',(0.,28.5,-0.3));
#8419=CARTESIAN_POINT('',(0.,0.,0.));
#8420=CARTESIAN_POINT('Origin',(-4.75,0.,1.2));
#8421=CARTESIAN_POINT('',(-5.175,-5.20474889637625E-17,2.4));
#8422=CARTESIAN_POINT('Origin',(-4.75,0.,2.4));
#8423=CARTESIAN_POINT('',(-5.175,-5.20474889637625E-17,1.2));
#8424=CARTESIAN_POINT('',(-5.175,-5.20474889637625E-17,1.2));
#8425=CARTESIAN_POINT('Origin',(-4.75,0.,1.2));
#8426=CARTESIAN_POINT('Origin',(-4.75,0.,1.2));
#8427=CARTESIAN_POINT('',(-5.395,-7.89897185450042E-17,2.4));
#8428=CARTESIAN_POINT('Origin',(-4.75,0.,2.4));
#8429=CARTESIAN_POINT('',(-5.395,-7.89897185450042E-17,1.2));
#8430=CARTESIAN_POINT('',(-5.395,-7.89897185450042E-17,1.2));
#8431=CARTESIAN_POINT('Origin',(-4.75,0.,1.2));
#8432=CARTESIAN_POINT('Origin',(-4.75,0.,2.4));
#8433=CARTESIAN_POINT('Origin',(-4.75,0.,1.2));
#8434=CARTESIAN_POINT('',(0.,0.,0.));
#8435=CARTESIAN_POINT('Origin',(4.75,0.,1.2));
#8436=CARTESIAN_POINT('',(4.325,-5.20474889637625E-17,2.4));
#8437=CARTESIAN_POINT('Origin',(4.75,0.,2.4));
#8438=CARTESIAN_POINT('',(4.325,-5.20474889637625E-17,1.2));
#8439=CARTESIAN_POINT('',(4.325,-5.20474889637625E-17,1.2));
#8440=CARTESIAN_POINT('Origin',(4.75,0.,1.2));
#8441=CARTESIAN_POINT('Origin',(4.75,0.,1.2));
#8442=CARTESIAN_POINT('',(4.105,-7.89897185450042E-17,2.4));
#8443=CARTESIAN_POINT('Origin',(4.75,0.,2.4));
#8444=CARTESIAN_POINT('',(4.105,-7.89897185450042E-17,1.2));
#8445=CARTESIAN_POINT('',(4.105,-7.89897185450042E-17,1.2));
#8446=CARTESIAN_POINT('Origin',(4.75,0.,1.2));
#8447=CARTESIAN_POINT('Origin',(4.75,0.,2.4));
#8448=CARTESIAN_POINT('Origin',(4.75,0.,1.2));
#8449=CARTESIAN_POINT('',(0.,0.,0.));
#8450=CARTESIAN_POINT('Origin',(-4.75,20.,1.2));
#8451=CARTESIAN_POINT('',(-5.175,20.,2.4));
#8452=CARTESIAN_POINT('Origin',(-4.75,20.,2.4));
#8453=CARTESIAN_POINT('',(-5.175,20.,1.2));
#8454=CARTESIAN_POINT('',(-5.175,20.,1.2));
#8455=CARTESIAN_POINT('Origin',(-4.75,20.,1.2));
#8456=CARTESIAN_POINT('Origin',(-4.75,20.,1.2));
#8457=CARTESIAN_POINT('',(-5.395,20.,2.4));
#8458=CARTESIAN_POINT('Origin',(-4.75,20.,2.4));
#8459=CARTESIAN_POINT('',(-5.395,20.,1.2));
#8460=CARTESIAN_POINT('',(-5.395,20.,1.2));
#8461=CARTESIAN_POINT('Origin',(-4.75,20.,1.2));
#8462=CARTESIAN_POINT('Origin',(-4.75,20.,2.4));
#8463=CARTESIAN_POINT('Origin',(-4.75,20.,1.2));
#8464=CARTESIAN_POINT('',(0.,0.,0.));
#8465=CARTESIAN_POINT('Origin',(4.75,20.,1.2));
#8466=CARTESIAN_POINT('',(4.325,20.,2.4));
#8467=CARTESIAN_POINT('Origin',(4.75,20.,2.4));
#8468=CARTESIAN_POINT('',(4.325,20.,1.2));
#8469=CARTESIAN_POINT('',(4.325,20.,1.2));
#8470=CARTESIAN_POINT('Origin',(4.75,20.,1.2));
#8471=CARTESIAN_POINT('Origin',(4.75,20.,1.2));
#8472=CARTESIAN_POINT('',(4.105,20.,2.4));
#8473=CARTESIAN_POINT('Origin',(4.75,20.,2.4));
#8474=CARTESIAN_POINT('',(4.105,20.,1.2));
#8475=CARTESIAN_POINT('',(4.105,20.,1.2));
#8476=CARTESIAN_POINT('Origin',(4.75,20.,1.2));
#8477=CARTESIAN_POINT('Origin',(4.75,20.,2.4));
#8478=CARTESIAN_POINT('Origin',(4.75,20.,1.2));
#8479=CARTESIAN_POINT('',(0.,0.,0.));
#8480=CARTESIAN_POINT('',(0.,0.,0.));
#8481=CARTESIAN_POINT('Origin',(0.,0.,0.));
#8482=CARTESIAN_POINT('',(-2.05,-1.65,2.51052593825207E-16));
#8483=CARTESIAN_POINT('Origin',(0.,-1.65,0.));
#8484=CARTESIAN_POINT('',(-2.05,-1.14891252930761,-2.51052593825207E-16));
#8485=CARTESIAN_POINT('',(-2.05,0.,2.51052593825207E-16));
#8486=CARTESIAN_POINT('Origin',(0.,-1.14891252930761,0.));
#8487=CARTESIAN_POINT('Origin',(0.,0.,0.));
#8488=CARTESIAN_POINT('',(-2.05,1.14891252930761,2.51052593825207E-16));
#8489=CARTESIAN_POINT('Origin',(0.,1.14891252930761,0.));
#8490=CARTESIAN_POINT('',(-2.05,1.65,-2.51052593825207E-16));
#8491=CARTESIAN_POINT('',(-2.05,0.,2.51052593825207E-16));
#8492=CARTESIAN_POINT('Origin',(0.,1.65,0.));
#8493=CARTESIAN_POINT('Origin',(0.,0.,0.));
#8494=CARTESIAN_POINT('',(-1.43895998899814E-16,-1.76221774462768E-32,-2.35));
#8495=CARTESIAN_POINT('',(-1.43895998899814E-16,-1.76221774462768E-32,2.35));
#8496=CARTESIAN_POINT('Origin',(0.,0.,0.));
#8497=CARTESIAN_POINT('Origin',(0.,1.55,-1.49));
#8498=CARTESIAN_POINT('',(-3.76384615384615,1.55,-2.13));
#8499=CARTESIAN_POINT('',(-1.81744325908679,1.55,-2.13));
#8500=CARTESIAN_POINT('',(0.,1.55,-2.13));
#8501=CARTESIAN_POINT('',(-2.46585583768694,1.55,-1.32648218523477));
#8502=CARTESIAN_POINT('',(-1.68,1.55,-0.84));
#8503=CARTESIAN_POINT('Origin',(0.,1.55,0.));
#8504=CARTESIAN_POINT('Origin',(0.,1.55,-1.49));
#8505=CARTESIAN_POINT('',(1.81744325908679,1.55,-2.13));
#8506=CARTESIAN_POINT('',(3.76384615384615,1.55,-2.13));
#8507=CARTESIAN_POINT('',(0.,1.55,-2.13));
#8508=CARTESIAN_POINT('',(2.46585583768694,1.55,-1.32648218523477));
#8509=CARTESIAN_POINT('Origin',(0.,1.55,0.));
#8510=CARTESIAN_POINT('',(3.78,1.55,-2.14));
#8511=CARTESIAN_POINT('Origin',(0.,-1.55,-1.49));
#8512=CARTESIAN_POINT('',(-1.81744325908679,-1.55,-2.13));
#8513=CARTESIAN_POINT('',(-3.76384615384615,-1.55,-2.13));
#8514=CARTESIAN_POINT('',(0.,-1.55,-2.13));
#8515=CARTESIAN_POINT('',(-2.46585583768694,-1.55,-1.32648218523477));
#8516=CARTESIAN_POINT('Origin',(0.,-1.55,0.));
#8517=CARTESIAN_POINT('',(-1.68,-1.55,-0.84));
#8518=CARTESIAN_POINT('Origin',(-3.78,0.,-2.14));
#8519=CARTESIAN_POINT('',(-3.76384615384615,0.,-2.13));
#8520=CARTESIAN_POINT('',(-2.46585583768694,0.,-1.32648218523477));
#8521=CARTESIAN_POINT('Origin',(0.,-1.55,-1.49));
#8522=CARTESIAN_POINT('',(3.76384615384615,-1.55,-2.13));
#8523=CARTESIAN_POINT('',(1.81744325908679,-1.55,-2.13));
#8524=CARTESIAN_POINT('',(0.,-1.55,-2.13));
#8525=CARTESIAN_POINT('',(2.46585583768694,-1.55,-1.32648218523477));
#8526=CARTESIAN_POINT('',(3.78,-1.55,-2.14));
#8527=CARTESIAN_POINT('Origin',(0.,-1.55,0.));
#8528=CARTESIAN_POINT('Origin',(1.68,0.,-0.84));
#8529=CARTESIAN_POINT('',(3.76384615384615,0.,-2.13));
#8530=CARTESIAN_POINT('',(2.46585583768694,0.,-1.32648218523477));
#8531=CARTESIAN_POINT('Origin',(0.,0.,-2.13));
#8532=CARTESIAN_POINT('',(-6.35,1.9,-2.13));
#8533=CARTESIAN_POINT('',(-6.35,-1.9,-2.13));
#8534=CARTESIAN_POINT('',(-6.35,1.9,-2.13));
#8535=CARTESIAN_POINT('',(6.35,-1.9,-2.13));
#8536=CARTESIAN_POINT('',(-6.35,-1.9,-2.13));
#8537=CARTESIAN_POINT('',(6.35,1.9,-2.13));
#8538=CARTESIAN_POINT('',(6.35,-1.9,-2.13));
#8539=CARTESIAN_POINT('',(6.35,1.9,-2.13));
#8540=CARTESIAN_POINT('',(4.1,7.9602041944578E-17,-2.13));
#8541=CARTESIAN_POINT('Origin',(4.75,0.,-2.13));
#8542=CARTESIAN_POINT('',(-5.4,7.9602041944578E-17,-2.13));
#8543=CARTESIAN_POINT('Origin',(-4.75,0.,-2.13));
#8544=CARTESIAN_POINT('',(1.81744325908679,-1.65,-2.13));
#8545=CARTESIAN_POINT('',(1.81744325908679,0.,-2.13));
#8546=CARTESIAN_POINT('',(-1.81744325908679,-1.65,-2.13));
#8547=CARTESIAN_POINT('',(0.,-1.65,-2.13));
#8548=CARTESIAN_POINT('',(-1.81744325908679,0.,-2.13));
#8549=CARTESIAN_POINT('',(-1.81744325908679,1.65,-2.13));
#8550=CARTESIAN_POINT('',(-1.81744325908679,0.,-2.13));
#8551=CARTESIAN_POINT('',(1.81744325908679,1.65,-2.13));
#8552=CARTESIAN_POINT('',(0.,1.65,-2.13));
#8553=CARTESIAN_POINT('',(1.81744325908679,0.,-2.13));
#8554=CARTESIAN_POINT('Origin',(0.,0.,0.));
#8555=CARTESIAN_POINT('Origin',(0.,1.65,0.));
#8556=CARTESIAN_POINT('Origin',(0.,-1.65,0.));
#8557=CARTESIAN_POINT('Origin',(0.,-1.65,0.));
#8558=CARTESIAN_POINT('Origin',(0.,1.65,0.));
#8559=CARTESIAN_POINT('Origin',(3.35,1.4,-3.33));
#8560=CARTESIAN_POINT('',(3.35,1.4,-3.33));
#8561=CARTESIAN_POINT('',(-3.35,1.4,-3.33));
#8562=CARTESIAN_POINT('',(1.675,1.4,-3.33));
#8563=CARTESIAN_POINT('',(3.35,1.4,-2.83));
#8564=CARTESIAN_POINT('',(3.35,1.4,-3.33));
#8565=CARTESIAN_POINT('',(-3.35,1.4,-2.83));
#8566=CARTESIAN_POINT('',(3.35,1.4,-2.83));
#8567=CARTESIAN_POINT('',(-3.35,1.4,-3.33));
#8568=CARTESIAN_POINT('Origin',(3.35,-1.4,-3.33));
#8569=CARTESIAN_POINT('',(3.35,-1.4,-3.33));
#8570=CARTESIAN_POINT('',(3.35,-0.7,-3.33));
#8571=CARTESIAN_POINT('',(3.35,-1.4,-2.83));
#8572=CARTESIAN_POINT('',(3.35,-1.4,-3.33));
#8573=CARTESIAN_POINT('',(3.35,-1.4,-2.83));
#8574=CARTESIAN_POINT('Origin',(-3.35,-1.4,-3.33));
#8575=CARTESIAN_POINT('',(-3.35,-1.4,-3.33));
#8576=CARTESIAN_POINT('',(-1.675,-1.4,-3.33));
#8577=CARTESIAN_POINT('',(-3.35,-1.4,-2.83));
#8578=CARTESIAN_POINT('',(-3.35,-1.4,-3.33));
#8579=CARTESIAN_POINT('',(-3.35,-1.4,-2.83));
#8580=CARTESIAN_POINT('Origin',(-3.35,1.4,-3.33));
#8581=CARTESIAN_POINT('',(-3.35,0.7,-3.33));
#8582=CARTESIAN_POINT('',(-3.35,1.4,-2.83));
#8583=CARTESIAN_POINT('Origin',(0.,0.,-2.83));
#8584=CARTESIAN_POINT('Origin',(-4.75,0.,-3.33));
#8585=CARTESIAN_POINT('',(-5.4,-7.9602041944578E-17,-3.33));
#8586=CARTESIAN_POINT('Origin',(-4.75,0.,-3.33));
#8587=CARTESIAN_POINT('',(-5.4,-7.9602041944578E-17,-3.33));
#8588=CARTESIAN_POINT('Origin',(4.75,0.,-3.33));
#8589=CARTESIAN_POINT('',(4.1,-7.9602041944578E-17,-3.33));
#8590=CARTESIAN_POINT('Origin',(4.75,0.,-3.33));
#8591=CARTESIAN_POINT('',(4.1,-7.9602041944578E-17,-3.33));
#8592=CARTESIAN_POINT('Origin',(6.35,1.9,-3.33));
#8593=CARTESIAN_POINT('',(6.35,1.9,-3.33));
#8594=CARTESIAN_POINT('',(-6.35,1.9,-3.33));
#8595=CARTESIAN_POINT('',(6.35,1.9,-3.33));
#8596=CARTESIAN_POINT('',(-6.35,1.9,-3.33));
#8597=CARTESIAN_POINT('',(6.35,1.9,-3.33));
#8598=CARTESIAN_POINT('Origin',(6.35,-1.9,-3.33));
#8599=CARTESIAN_POINT('',(6.35,-1.9,-3.33));
#8600=CARTESIAN_POINT('',(6.35,-1.9,-3.33));
#8601=CARTESIAN_POINT('',(6.35,-1.9,-3.33));
#8602=CARTESIAN_POINT('Origin',(-6.35,-1.9,-3.33));
#8603=CARTESIAN_POINT('',(-6.35,-1.9,-3.33));
#8604=CARTESIAN_POINT('',(-6.35,-1.9,-3.33));
#8605=CARTESIAN_POINT('',(-6.35,-1.9,-3.33));
#8606=CARTESIAN_POINT('Origin',(-6.35,1.9,-3.33));
#8607=CARTESIAN_POINT('',(-6.35,1.9,-3.33));
#8608=CARTESIAN_POINT('Origin',(0.,0.,-3.33));
#8609=CARTESIAN_POINT('',(0.,0.,0.));
#8610=CARTESIAN_POINT('Origin',(0.,0.,0.));
#8611=CARTESIAN_POINT('',(-1.8,-0.85,-2.20436423846524E-16));
#8612=CARTESIAN_POINT('Origin',(0.,-0.85,0.));
#8613=CARTESIAN_POINT('',(-1.8,0.85,-2.20436423846524E-16));
#8614=CARTESIAN_POINT('',(-1.8,0.,-2.20436423846524E-16));
#8615=CARTESIAN_POINT('Origin',(0.,0.85,0.));
#8616=CARTESIAN_POINT('Origin',(2.19089023002066,0.85,0.));
#8617=CARTESIAN_POINT('',(2.19089023002066,0.85,0.));
#8618=CARTESIAN_POINT('Origin',(0.,0.85,0.));
#8619=CARTESIAN_POINT('Origin',(3.99680288865056E-15,0.,0.));
#8620=CARTESIAN_POINT('',(3.85290688975075E-15,-1.76221774462768E-32,2.35));
#8621=CARTESIAN_POINT('',(3.85290688975075E-15,-1.76221774462768E-32,-2.35));
#8622=CARTESIAN_POINT('Origin',(3.99680288865056E-15,0.,0.));
#8623=CARTESIAN_POINT('',(2.19089023002066,-0.85,0.));
#8624=CARTESIAN_POINT('Origin',(0.,-0.85,0.));
#8625=CARTESIAN_POINT('Origin',(1.8,-0.85,0.));
#8626=CARTESIAN_POINT('Origin',(0.,1.55,0.));
#8627=CARTESIAN_POINT('',(1.42894191624432,1.8,0.825000000000001));
#8628=CARTESIAN_POINT('',(1.53744468918255,1.55,0.598968970568896));
#8629=CARTESIAN_POINT('Ctrl Pts',(1.42894191624432,1.8,0.825000000000001));
#8630=CARTESIAN_POINT('Ctrl Pts',(1.44466308895875,1.8,0.797770130104052));
#8631=CARTESIAN_POINT('Ctrl Pts',(1.46055812562105,1.79370633789704,0.768258557763732));
#8632=CARTESIAN_POINT('Ctrl Pts',(1.48824888379079,1.76817777258318,0.713138492740816));
#8633=CARTESIAN_POINT('Ctrl Pts',(1.50008999307766,1.74894552961493,0.687551581002689));
#8634=CARTESIAN_POINT('Ctrl Pts',(1.51812136280714,1.70460745840382,0.646764802471699));
#8635=CARTESIAN_POINT('Ctrl Pts',(1.52552758004446,1.67652816181843,0.628833667319578));
#8636=CARTESIAN_POINT('Ctrl Pts',(1.53516661651472,1.61494799959182,0.604921184808251));
#8637=CARTESIAN_POINT('Ctrl Pts',(1.53744468918255,1.58144291640553,0.598968970568896));
#8638=CARTESIAN_POINT('Ctrl Pts',(1.53744468918255,1.55,0.598968970568896));
#8639=CARTESIAN_POINT('',(1.42894191624432,1.3,0.825000000000001));
#8640=CARTESIAN_POINT('Ctrl Pts',(1.42894191624432,1.3,0.825000000000001));
#8641=CARTESIAN_POINT('Ctrl Pts',(1.4132207435299,1.3,0.852229869895949));
#8642=CARTESIAN_POINT('Ctrl Pts',(1.39561049050871,1.30629366210296,0.880751161609749));
#8643=CARTESIAN_POINT('Ctrl Pts',(1.36172049302549,1.33182222741682,0.932292094146256));
#8644=CARTESIAN_POINT('Ctrl Pts',(1.34548213209931,1.35105447038507,0.955340251466734));
#8645=CARTESIAN_POINT('Ctrl Pts',(1.31917543061769,1.39539254159618,0.99134926498299));
#8646=CARTESIAN_POINT('Ctrl Pts',(1.30734972067592,1.42347183818157,1.00672880483252));
#8647=CARTESIAN_POINT('Ctrl Pts',(1.29146042158868,1.48505200040818,1.02703269653942));
#8648=CARTESIAN_POINT('Ctrl Pts',(1.28744468918255,1.51855708359447,1.03198167246111));
#8649=CARTESIAN_POINT('Ctrl Pts',(1.28744468918255,1.58144291640553,1.03198167246111));
#8650=CARTESIAN_POINT('Ctrl Pts',(1.29146042158868,1.61494799959182,1.02703269653942));
#8651=CARTESIAN_POINT('Ctrl Pts',(1.30734972067592,1.67652816181843,1.00672880483252));
#8652=CARTESIAN_POINT('Ctrl Pts',(1.31917543061769,1.70460745840382,0.991349264982991));
#8653=CARTESIAN_POINT('Ctrl Pts',(1.34548213209931,1.74894552961493,0.955340251466735));
#8654=CARTESIAN_POINT('Ctrl Pts',(1.36172049302549,1.76817777258318,0.932292094146256));
#8655=CARTESIAN_POINT('Ctrl Pts',(1.39561049050871,1.79370633789704,0.880751161609749));
#8656=CARTESIAN_POINT('Ctrl Pts',(1.4132207435299,1.8,0.85222986989595));
#8657=CARTESIAN_POINT('Ctrl Pts',(1.42894191624432,1.8,0.825000000000001));
#8658=CARTESIAN_POINT('Ctrl Pts',(1.53744468918255,1.55,0.598968970568896));
#8659=CARTESIAN_POINT('Ctrl Pts',(1.53744468918255,1.51855708359447,0.598968970568896));
#8660=CARTESIAN_POINT('Ctrl Pts',(1.53516661651472,1.48505200040818,0.60492118480825));
#8661=CARTESIAN_POINT('Ctrl Pts',(1.52552758004446,1.42347183818157,0.628833667319578));
#8662=CARTESIAN_POINT('Ctrl Pts',(1.51812136280714,1.39539254159618,0.646764802471699));
#8663=CARTESIAN_POINT('Ctrl Pts',(1.50008999307766,1.35105447038507,0.687551581002689));
#8664=CARTESIAN_POINT('Ctrl Pts',(1.48824888379079,1.33182222741682,0.713138492740816));
#8665=CARTESIAN_POINT('Ctrl Pts',(1.46055812562105,1.30629366210296,0.768258557763732));
#8666=CARTESIAN_POINT('Ctrl Pts',(1.44466308895875,1.3,0.797770130104052));
#8667=CARTESIAN_POINT('Ctrl Pts',(1.42894191624432,1.3,0.825000000000001));
#8668=CARTESIAN_POINT('',(0.963525491562421,1.55,0.267616567329818));
#8669=CARTESIAN_POINT('',(0.125,1.55,-0.21650635094611));
#8670=CARTESIAN_POINT('Ctrl Pts',(0.963525491562421,1.55,0.267616567329818));
#8671=CARTESIAN_POINT('Ctrl Pts',(0.963525491562421,1.5815373526696,0.267616567329818));
#8672=CARTESIAN_POINT('Ctrl Pts',(0.961833761492987,1.61508042700263,0.273949373987484));
#8673=CARTESIAN_POINT('Ctrl Pts',(0.954308486908894,1.67663267125761,0.299111603474268));
#8674=CARTESIAN_POINT('Ctrl Pts',(0.948394987258249,1.70465411363682,0.31788699900678));
#8675=CARTESIAN_POINT('Ctrl Pts',(0.933155485613026,1.74889618382539,0.360174810895352));
#8676=CARTESIAN_POINT('Ctrl Pts',(0.92278792026947,1.76811531482682,0.386546956384144));
#8677=CARTESIAN_POINT('Ctrl Pts',(0.897143218189782,1.79367084275751,0.442820664919227));
#8678=CARTESIAN_POINT('Ctrl Pts',(0.881791875377343,1.8,0.472691670144998));
#8679=CARTESIAN_POINT('Ctrl Pts',(0.850258932191534,1.8,0.527308329855003));
#8680=CARTESIAN_POINT('Ctrl Pts',(0.832065554235658,1.79367084275751,0.555538485325664));
#8681=CARTESIAN_POINT('Ctrl Pts',(0.796153444118959,1.76811531482682,0.605884303066698));
#8682=CARTESIAN_POINT('Ctrl Pts',(0.778498278845144,1.74889618382539,0.62804895077401));
#8683=CARTESIAN_POINT('Ctrl Pts',(0.749495710301794,1.70465411363682,0.662390652284073));
#8684=CARTESIAN_POINT('Ctrl Pts',(0.73619249062986,1.67663267125761,0.676899590973058));
#8685=CARTESIAN_POINT('Ctrl Pts',(0.718163997970498,1.61508042700263,0.695997784676728));
#8686=CARTESIAN_POINT('Ctrl Pts',(0.713525491562421,1.5815373526696,0.700629269222037));
#8687=CARTESIAN_POINT('Ctrl Pts',(0.713525491562421,1.5184626473304,0.700629269222037));
#8688=CARTESIAN_POINT('Ctrl Pts',(0.718163997970498,1.48491957299737,0.695997784676728));
#8689=CARTESIAN_POINT('Ctrl Pts',(0.73619249062986,1.42336732874239,0.676899590973058));
#8690=CARTESIAN_POINT('Ctrl Pts',(0.749495710301794,1.39534588636318,0.662390652284073));
#8691=CARTESIAN_POINT('Ctrl Pts',(0.778498278845144,1.35110381617461,0.62804895077401));
#8692=CARTESIAN_POINT('Ctrl Pts',(0.796153444118959,1.33188468517318,0.605884303066698));
#8693=CARTESIAN_POINT('Ctrl Pts',(0.832065554235658,1.30632915724249,0.555538485325664));
#8694=CARTESIAN_POINT('Ctrl Pts',(0.850258932191534,1.3,0.527308329855003));
#8695=CARTESIAN_POINT('Ctrl Pts',(0.881791875377343,1.3,0.472691670144998));
#8696=CARTESIAN_POINT('Ctrl Pts',(0.897143218189782,1.30632915724249,0.442820664919227));
#8697=CARTESIAN_POINT('Ctrl Pts',(0.92278792026947,1.33188468517318,0.386546956384144));
#8698=CARTESIAN_POINT('Ctrl Pts',(0.933155485613026,1.35110381617461,0.360174810895352));
#8699=CARTESIAN_POINT('Ctrl Pts',(0.948394987258249,1.39534588636318,0.31788699900678));
#8700=CARTESIAN_POINT('Ctrl Pts',(0.954308486908894,1.42336732874239,0.299111603474268));
#8701=CARTESIAN_POINT('Ctrl Pts',(0.961833761492987,1.48491957299738,0.273949373987484));
#8702=CARTESIAN_POINT('Ctrl Pts',(0.963525491562421,1.5184626473304,0.267616567329818));
#8703=CARTESIAN_POINT('Ctrl Pts',(0.963525491562421,1.55,0.267616567329818));
#8704=CARTESIAN_POINT('Origin',(0.,1.55,0.));
#8705=CARTESIAN_POINT('',(-0.713525491562421,1.55,-0.700629269222037));
#8706=CARTESIAN_POINT('Ctrl Pts',(-0.713525491562421,1.55,-0.700629269222037));
#8707=CARTESIAN_POINT('Ctrl Pts',(-0.713525491562421,1.5184626473304,-0.700629269222037));
#8708=CARTESIAN_POINT('Ctrl Pts',(-0.718163997970498,1.48491957299737,-0.695997784676728));
#8709=CARTESIAN_POINT('Ctrl Pts',(-0.73619249062986,1.42336732874239,-0.676899590973058));
#8710=CARTESIAN_POINT('Ctrl Pts',(-0.749495710301794,1.39534588636318,-0.662390652284073));
#8711=CARTESIAN_POINT('Ctrl Pts',(-0.778498278845144,1.35110381617461,-0.62804895077401));
#8712=CARTESIAN_POINT('Ctrl Pts',(-0.796153444118959,1.33188468517318,-0.605884303066698));
#8713=CARTESIAN_POINT('Ctrl Pts',(-0.832065554235658,1.30632915724249,-0.555538485325664));
#8714=CARTESIAN_POINT('Ctrl Pts',(-0.850258932191534,1.3,-0.527308329855003));
#8715=CARTESIAN_POINT('Ctrl Pts',(-0.881791875377343,1.3,-0.472691670144998));
#8716=CARTESIAN_POINT('Ctrl Pts',(-0.897143218189782,1.30632915724249,-0.442820664919227));
#8717=CARTESIAN_POINT('Ctrl Pts',(-0.92278792026947,1.33188468517318,-0.386546956384144));
#8718=CARTESIAN_POINT('Ctrl Pts',(-0.933155485613026,1.35110381617461,-0.360174810895352));
#8719=CARTESIAN_POINT('Ctrl Pts',(-0.948394987258249,1.39534588636318,-0.31788699900678));
#8720=CARTESIAN_POINT('Ctrl Pts',(-0.954308486908894,1.42336732874239,-0.299111603474268));
#8721=CARTESIAN_POINT('Ctrl Pts',(-0.961833761492986,1.48491957299737,-0.273949373987484));
#8722=CARTESIAN_POINT('Ctrl Pts',(-0.963525491562421,1.5184626473304,-0.267616567329818));
#8723=CARTESIAN_POINT('Ctrl Pts',(-0.963525491562421,1.5815373526696,-0.267616567329818));
#8724=CARTESIAN_POINT('Ctrl Pts',(-0.961833761492986,1.61508042700263,-0.273949373987484));
#8725=CARTESIAN_POINT('Ctrl Pts',(-0.954308486908894,1.67663267125761,-0.299111603474268));
#8726=CARTESIAN_POINT('Ctrl Pts',(-0.948394987258249,1.70465411363682,-0.31788699900678));
#8727=CARTESIAN_POINT('Ctrl Pts',(-0.933155485613026,1.74889618382539,-0.360174810895352));
#8728=CARTESIAN_POINT('Ctrl Pts',(-0.92278792026947,1.76811531482682,-0.386546956384144));
#8729=CARTESIAN_POINT('Ctrl Pts',(-0.897143218189782,1.79367084275751,-0.442820664919227));
#8730=CARTESIAN_POINT('Ctrl Pts',(-0.881791875377343,1.8,-0.472691670144998));
#8731=CARTESIAN_POINT('Ctrl Pts',(-0.850258932191534,1.8,-0.527308329855003));
#8732=CARTESIAN_POINT('Ctrl Pts',(-0.832065554235658,1.79367084275751,-0.555538485325664));
#8733=CARTESIAN_POINT('Ctrl Pts',(-0.796153444118959,1.76811531482682,-0.605884303066698));
#8734=CARTESIAN_POINT('Ctrl Pts',(-0.778498278845144,1.74889618382539,-0.62804895077401));
#8735=CARTESIAN_POINT('Ctrl Pts',(-0.749495710301794,1.70465411363682,-0.662390652284073));
#8736=CARTESIAN_POINT('Ctrl Pts',(-0.73619249062986,1.67663267125761,-0.676899590973058));
#8737=CARTESIAN_POINT('Ctrl Pts',(-0.718163997970498,1.61508042700263,-0.695997784676728));
#8738=CARTESIAN_POINT('Ctrl Pts',(-0.713525491562421,1.5815373526696,-0.700629269222037));
#8739=CARTESIAN_POINT('Ctrl Pts',(-0.713525491562421,1.55,-0.700629269222037));
#8740=CARTESIAN_POINT('',(-1.28744468918255,1.55,-1.03198167246111));
#8741=CARTESIAN_POINT('',(0.125,1.55,-0.21650635094611));
#8742=CARTESIAN_POINT('',(-1.42894191624432,1.3,-0.825000000000001));
#8743=CARTESIAN_POINT('Ctrl Pts',(-1.42894191624432,1.3,-0.825000000000001));
#8744=CARTESIAN_POINT('Ctrl Pts',(-1.4132207435299,1.3,-0.852229869895949));
#8745=CARTESIAN_POINT('Ctrl Pts',(-1.39561049050871,1.30629366210296,-0.880751161609749));
#8746=CARTESIAN_POINT('Ctrl Pts',(-1.36172049302549,1.33182222741682,-0.932292094146256));
#8747=CARTESIAN_POINT('Ctrl Pts',(-1.34548213209931,1.35105447038507,-0.955340251466735));
#8748=CARTESIAN_POINT('Ctrl Pts',(-1.31917543061769,1.39539254159618,-0.991349264982991));
#8749=CARTESIAN_POINT('Ctrl Pts',(-1.30734972067592,1.42347183818157,-1.00672880483252));
#8750=CARTESIAN_POINT('Ctrl Pts',(-1.29146042158868,1.48505200040818,-1.02703269653942));
#8751=CARTESIAN_POINT('Ctrl Pts',(-1.28744468918255,1.51855708359447,-1.03198167246111));
#8752=CARTESIAN_POINT('Ctrl Pts',(-1.28744468918255,1.55,-1.03198167246111));
#8753=CARTESIAN_POINT('',(-1.42894191624432,1.8,-0.825000000000001));
#8754=CARTESIAN_POINT('Ctrl Pts',(-1.42894191624432,1.8,-0.825000000000001));
#8755=CARTESIAN_POINT('Ctrl Pts',(-1.44466308895875,1.8,-0.797770130104052));
#8756=CARTESIAN_POINT('Ctrl Pts',(-1.46055812562105,1.79370633789704,-0.768258557763732));
#8757=CARTESIAN_POINT('Ctrl Pts',(-1.48824888379079,1.76817777258318,-0.713138492740816));
#8758=CARTESIAN_POINT('Ctrl Pts',(-1.50008999307766,1.74894552961493,-0.687551581002689));
#8759=CARTESIAN_POINT('Ctrl Pts',(-1.51812136280714,1.70460745840382,-0.646764802471699));
#8760=CARTESIAN_POINT('Ctrl Pts',(-1.52552758004446,1.67652816181843,-0.628833667319578));
#8761=CARTESIAN_POINT('Ctrl Pts',(-1.53516661651472,1.61494799959182,-0.60492118480825));
#8762=CARTESIAN_POINT('Ctrl Pts',(-1.53744468918255,1.58144291640553,-0.598968970568896));
#8763=CARTESIAN_POINT('Ctrl Pts',(-1.53744468918255,1.51855708359447,-0.598968970568896));
#8764=CARTESIAN_POINT('Ctrl Pts',(-1.53516661651472,1.48505200040818,-0.60492118480825));
#8765=CARTESIAN_POINT('Ctrl Pts',(-1.52552758004446,1.42347183818157,-0.628833667319578));
#8766=CARTESIAN_POINT('Ctrl Pts',(-1.51812136280714,1.39539254159618,-0.646764802471699));
#8767=CARTESIAN_POINT('Ctrl Pts',(-1.50008999307766,1.35105447038507,-0.687551581002689));
#8768=CARTESIAN_POINT('Ctrl Pts',(-1.48824888379079,1.33182222741682,-0.713138492740816));
#8769=CARTESIAN_POINT('Ctrl Pts',(-1.46055812562105,1.30629366210296,-0.768258557763732));
#8770=CARTESIAN_POINT('Ctrl Pts',(-1.44466308895875,1.3,-0.797770130104052));
#8771=CARTESIAN_POINT('Ctrl Pts',(-1.42894191624432,1.3,-0.825000000000001));
#8772=CARTESIAN_POINT('Ctrl Pts',(-1.28744468918255,1.55,-1.03198167246111));
#8773=CARTESIAN_POINT('Ctrl Pts',(-1.28744468918255,1.58144291640553,-1.03198167246111));
#8774=CARTESIAN_POINT('Ctrl Pts',(-1.29146042158868,1.61494799959182,-1.02703269653942));
#8775=CARTESIAN_POINT('Ctrl Pts',(-1.30734972067592,1.67652816181843,-1.00672880483252));
#8776=CARTESIAN_POINT('Ctrl Pts',(-1.31917543061769,1.70460745840382,-0.991349264982991));
#8777=CARTESIAN_POINT('Ctrl Pts',(-1.34548213209931,1.74894552961493,-0.955340251466734));
#8778=CARTESIAN_POINT('Ctrl Pts',(-1.36172049302549,1.76817777258318,-0.932292094146256));
#8779=CARTESIAN_POINT('Ctrl Pts',(-1.39561049050871,1.79370633789704,-0.880751161609749));
#8780=CARTESIAN_POINT('Ctrl Pts',(-1.4132207435299,1.8,-0.852229869895949));
#8781=CARTESIAN_POINT('Ctrl Pts',(-1.42894191624432,1.8,-0.825000000000001));
#8782=CARTESIAN_POINT('Origin',(0.,1.55,0.));
#8783=CARTESIAN_POINT('',(-1.65,0.85,-2.02066721859313E-16));
#8784=CARTESIAN_POINT('Origin',(0.,0.85,0.));
#8785=CARTESIAN_POINT('',(-1.65,2.25,-2.02066721859313E-16));
#8786=CARTESIAN_POINT('',(-1.65,1.55,-2.02066721859313E-16));
#8787=CARTESIAN_POINT('Origin',(0.,2.25,0.));
#8788=CARTESIAN_POINT('',(-1.42894191624432,1.3,0.825));
#8789=CARTESIAN_POINT('',(-1.42894191624432,1.8,0.825));
#8790=CARTESIAN_POINT('Ctrl Pts',(-1.42894191624432,1.3,0.825));
#8791=CARTESIAN_POINT('Ctrl Pts',(-1.44466308895875,1.3,0.797770130104051));
#8792=CARTESIAN_POINT('Ctrl Pts',(-1.46055812562105,1.30629366210296,0.768258557763731));
#8793=CARTESIAN_POINT('Ctrl Pts',(-1.48824888379079,1.33182222741682,0.713138492740815));
#8794=CARTESIAN_POINT('Ctrl Pts',(-1.50008999307766,1.35105447038507,0.687551581002688));
#8795=CARTESIAN_POINT('Ctrl Pts',(-1.51812136280714,1.39539254159618,0.646764802471698));
#8796=CARTESIAN_POINT('Ctrl Pts',(-1.52552758004446,1.42347183818157,0.628833667319577));
#8797=CARTESIAN_POINT('Ctrl Pts',(-1.53516661651472,1.48505200040818,0.604921184808249));
#8798=CARTESIAN_POINT('Ctrl Pts',(-1.53744468918255,1.51855708359447,0.598968970568895));
#8799=CARTESIAN_POINT('Ctrl Pts',(-1.53744468918255,1.58144291640553,0.598968970568895));
#8800=CARTESIAN_POINT('Ctrl Pts',(-1.53516661651472,1.61494799959182,0.604921184808249));
#8801=CARTESIAN_POINT('Ctrl Pts',(-1.52552758004446,1.67652816181843,0.628833667319577));
#8802=CARTESIAN_POINT('Ctrl Pts',(-1.51812136280714,1.70460745840382,0.646764802471698));
#8803=CARTESIAN_POINT('Ctrl Pts',(-1.50008999307766,1.74894552961493,0.687551581002688));
#8804=CARTESIAN_POINT('Ctrl Pts',(-1.48824888379079,1.76817777258318,0.713138492740815));
#8805=CARTESIAN_POINT('Ctrl Pts',(-1.46055812562105,1.79370633789704,0.768258557763731));
#8806=CARTESIAN_POINT('Ctrl Pts',(-1.44466308895875,1.8,0.797770130104051));
#8807=CARTESIAN_POINT('Ctrl Pts',(-1.42894191624432,1.8,0.825));
#8808=CARTESIAN_POINT('',(-1.28744468918255,1.55,1.03198167246111));
#8809=CARTESIAN_POINT('Ctrl Pts',(-1.42894191624432,1.8,0.825));
#8810=CARTESIAN_POINT('Ctrl Pts',(-1.4132207435299,1.8,0.852229869895948));
#8811=CARTESIAN_POINT('Ctrl Pts',(-1.39561049050871,1.79370633789704,0.880751161609747));
#8812=CARTESIAN_POINT('Ctrl Pts',(-1.36172049302549,1.76817777258318,0.932292094146255));
#8813=CARTESIAN_POINT('Ctrl Pts',(-1.34548213209931,1.74894552961493,0.955340251466733));
#8814=CARTESIAN_POINT('Ctrl Pts',(-1.31917543061769,1.70460745840382,0.991349264982989));
#8815=CARTESIAN_POINT('Ctrl Pts',(-1.30734972067592,1.67652816181843,1.00672880483252));
#8816=CARTESIAN_POINT('Ctrl Pts',(-1.29146042158868,1.61494799959182,1.02703269653942));
#8817=CARTESIAN_POINT('Ctrl Pts',(-1.28744468918255,1.58144291640553,1.03198167246111));
#8818=CARTESIAN_POINT('Ctrl Pts',(-1.28744468918255,1.55,1.03198167246111));
#8819=CARTESIAN_POINT('Ctrl Pts',(-1.28744468918255,1.55,1.03198167246111));
#8820=CARTESIAN_POINT('Ctrl Pts',(-1.28744468918255,1.51855708359447,1.03198167246111));
#8821=CARTESIAN_POINT('Ctrl Pts',(-1.29146042158868,1.48505200040818,1.02703269653942));
#8822=CARTESIAN_POINT('Ctrl Pts',(-1.30734972067592,1.42347183818157,1.00672880483252));
#8823=CARTESIAN_POINT('Ctrl Pts',(-1.31917543061769,1.39539254159618,0.99134926498299));
#8824=CARTESIAN_POINT('Ctrl Pts',(-1.34548213209931,1.35105447038508,0.955340251466733));
#8825=CARTESIAN_POINT('Ctrl Pts',(-1.36172049302549,1.33182222741682,0.932292094146255));
#8826=CARTESIAN_POINT('Ctrl Pts',(-1.39561049050871,1.30629366210296,0.880751161609748));
#8827=CARTESIAN_POINT('Ctrl Pts',(-1.4132207435299,1.3,0.852229869895949));
#8828=CARTESIAN_POINT('Ctrl Pts',(-1.42894191624432,1.3,0.825));
#8829=CARTESIAN_POINT('',(1.42894191624432,1.8,-0.825));
#8830=CARTESIAN_POINT('',(1.42894191624432,1.3,-0.825));
#8831=CARTESIAN_POINT('Ctrl Pts',(1.42894191624432,1.8,-0.825));
#8832=CARTESIAN_POINT('Ctrl Pts',(1.4132207435299,1.8,-0.852229869895949));
#8833=CARTESIAN_POINT('Ctrl Pts',(1.39561049050871,1.79370633789704,-0.880751161609748));
#8834=CARTESIAN_POINT('Ctrl Pts',(1.36172049302549,1.76817777258318,-0.932292094146255));
#8835=CARTESIAN_POINT('Ctrl Pts',(1.34548213209931,1.74894552961493,-0.955340251466734));
#8836=CARTESIAN_POINT('Ctrl Pts',(1.31917543061769,1.70460745840382,-0.99134926498299));
#8837=CARTESIAN_POINT('Ctrl Pts',(1.30734972067592,1.67652816181843,-1.00672880483252));
#8838=CARTESIAN_POINT('Ctrl Pts',(1.29146042158868,1.61494799959182,-1.02703269653942));
#8839=CARTESIAN_POINT('Ctrl Pts',(1.28744468918255,1.58144291640553,-1.03198167246111));
#8840=CARTESIAN_POINT('Ctrl Pts',(1.28744468918255,1.51855708359447,-1.03198167246111));
#8841=CARTESIAN_POINT('Ctrl Pts',(1.29146042158868,1.48505200040818,-1.02703269653942));
#8842=CARTESIAN_POINT('Ctrl Pts',(1.30734972067592,1.42347183818157,-1.00672880483252));
#8843=CARTESIAN_POINT('Ctrl Pts',(1.31917543061769,1.39539254159618,-0.99134926498299));
#8844=CARTESIAN_POINT('Ctrl Pts',(1.34548213209931,1.35105447038507,-0.955340251466734));
#8845=CARTESIAN_POINT('Ctrl Pts',(1.36172049302549,1.33182222741682,-0.932292094146255));
#8846=CARTESIAN_POINT('Ctrl Pts',(1.39561049050871,1.30629366210296,-0.880751161609748));
#8847=CARTESIAN_POINT('Ctrl Pts',(1.4132207435299,1.3,-0.852229869895948));
#8848=CARTESIAN_POINT('Ctrl Pts',(1.42894191624432,1.3,-0.825));
#8849=CARTESIAN_POINT('',(1.53744468918255,1.55,-0.598968970568895));
#8850=CARTESIAN_POINT('Ctrl Pts',(1.42894191624432,1.3,-0.825));
#8851=CARTESIAN_POINT('Ctrl Pts',(1.44466308895875,1.3,-0.797770130104051));
#8852=CARTESIAN_POINT('Ctrl Pts',(1.46055812562105,1.30629366210296,-0.768258557763731));
#8853=CARTESIAN_POINT('Ctrl Pts',(1.48824888379079,1.33182222741682,-0.713138492740815));
#8854=CARTESIAN_POINT('Ctrl Pts',(1.50008999307766,1.35105447038507,-0.687551581002688));
#8855=CARTESIAN_POINT('Ctrl Pts',(1.51812136280714,1.39539254159618,-0.646764802471698));
#8856=CARTESIAN_POINT('Ctrl Pts',(1.52552758004446,1.42347183818157,-0.628833667319577));
#8857=CARTESIAN_POINT('Ctrl Pts',(1.53516661651472,1.48505200040818,-0.604921184808249));
#8858=CARTESIAN_POINT('Ctrl Pts',(1.53744468918255,1.51855708359447,-0.598968970568895));
#8859=CARTESIAN_POINT('Ctrl Pts',(1.53744468918255,1.55,-0.598968970568895));
#8860=CARTESIAN_POINT('Ctrl Pts',(1.53744468918255,1.55,-0.598968970568895));
#8861=CARTESIAN_POINT('Ctrl Pts',(1.53744468918255,1.58144291640553,-0.598968970568895));
#8862=CARTESIAN_POINT('Ctrl Pts',(1.53516661651472,1.61494799959182,-0.604921184808249));
#8863=CARTESIAN_POINT('Ctrl Pts',(1.52552758004446,1.67652816181843,-0.628833667319577));
#8864=CARTESIAN_POINT('Ctrl Pts',(1.51812136280714,1.70460745840382,-0.646764802471698));
#8865=CARTESIAN_POINT('Ctrl Pts',(1.50008999307766,1.74894552961493,-0.687551581002688));
#8866=CARTESIAN_POINT('Ctrl Pts',(1.48824888379079,1.76817777258318,-0.713138492740815));
#8867=CARTESIAN_POINT('Ctrl Pts',(1.46055812562105,1.79370633789704,-0.768258557763731));
#8868=CARTESIAN_POINT('Ctrl Pts',(1.44466308895875,1.8,-0.797770130104051));
#8869=CARTESIAN_POINT('Ctrl Pts',(1.42894191624432,1.8,-0.825));
#8870=CARTESIAN_POINT('',(0.,1.3,-1.65));
#8871=CARTESIAN_POINT('',(0.,1.8,-1.65));
#8872=CARTESIAN_POINT('Ctrl Pts',(1.38777878078145E-17,1.3,-1.65));
#8873=CARTESIAN_POINT('Ctrl Pts',(0.0314423454288489,1.3,-1.65));
#8874=CARTESIAN_POINT('Ctrl Pts',(0.0649476351123396,1.30629366210296,-1.64900971937348));
#8875=CARTESIAN_POINT('Ctrl Pts',(0.126528390765307,1.33182222741682,-1.64543058688707));
#8876=CARTESIAN_POINT('Ctrl Pts',(0.154607860978348,1.35105447038507,-1.64289183246942));
#8877=CARTESIAN_POINT('Ctrl Pts',(0.198945932189457,1.39539254159618,-1.63811406745469));
#8878=CARTESIAN_POINT('Ctrl Pts',(0.218177859368546,1.42347183818157,-1.63556247215209));
#8879=CARTESIAN_POINT('Ctrl Pts',(0.243706194926033,1.48505200040818,-1.63195388134767));
#8880=CARTESIAN_POINT('Ctrl Pts',(0.25,1.51855708359447,-1.63095064303001));
#8881=CARTESIAN_POINT('Ctrl Pts',(0.25,1.58144291640553,-1.63095064303001));
#8882=CARTESIAN_POINT('Ctrl Pts',(0.243706194926033,1.61494799959182,-1.63195388134767));
#8883=CARTESIAN_POINT('Ctrl Pts',(0.218177859368546,1.67652816181843,-1.63556247215209));
#8884=CARTESIAN_POINT('Ctrl Pts',(0.198945932189457,1.70460745840382,-1.63811406745469));
#8885=CARTESIAN_POINT('Ctrl Pts',(0.154607860978349,1.74894552961493,-1.64289183246942));
#8886=CARTESIAN_POINT('Ctrl Pts',(0.126528390765307,1.76817777258318,-1.64543058688707));
#8887=CARTESIAN_POINT('Ctrl Pts',(0.0649476351123398,1.79370633789704,-1.64900971937348));
#8888=CARTESIAN_POINT('Ctrl Pts',(0.031442345428849,1.8,-1.65));
#8889=CARTESIAN_POINT('Ctrl Pts',(7.63278329429795E-17,1.8,-1.65));
#8890=CARTESIAN_POINT('',(-0.25,1.55,-1.63095064303001));
#8891=CARTESIAN_POINT('Ctrl Pts',(9.0205620750794E-17,1.8,-1.65));
#8892=CARTESIAN_POINT('Ctrl Pts',(-0.0314423454288488,1.8,-1.65));
#8893=CARTESIAN_POINT('Ctrl Pts',(-0.0649476351123396,1.79370633789704,
-1.64900971937348));
#8894=CARTESIAN_POINT('Ctrl Pts',(-0.126528390765307,1.76817777258318,-1.64543058688707));
#8895=CARTESIAN_POINT('Ctrl Pts',(-0.154607860978348,1.74894552961493,-1.64289183246942));
#8896=CARTESIAN_POINT('Ctrl Pts',(-0.198945932189456,1.70460745840382,-1.63811406745469));
#8897=CARTESIAN_POINT('Ctrl Pts',(-0.218177859368546,1.67652816181843,-1.63556247215209));
#8898=CARTESIAN_POINT('Ctrl Pts',(-0.243706194926033,1.61494799959182,-1.63195388134767));
#8899=CARTESIAN_POINT('Ctrl Pts',(-0.25,1.58144291640553,-1.63095064303001));
#8900=CARTESIAN_POINT('Ctrl Pts',(-0.25,1.55,-1.63095064303001));
#8901=CARTESIAN_POINT('Ctrl Pts',(-0.25,1.55,-1.63095064303001));
#8902=CARTESIAN_POINT('Ctrl Pts',(-0.25,1.51855708359447,-1.63095064303001));
#8903=CARTESIAN_POINT('Ctrl Pts',(-0.243706194926033,1.48505200040818,-1.63195388134767));
#8904=CARTESIAN_POINT('Ctrl Pts',(-0.218177859368546,1.42347183818157,-1.63556247215209));
#8905=CARTESIAN_POINT('Ctrl Pts',(-0.198945932189457,1.39539254159618,-1.63811406745469));
#8906=CARTESIAN_POINT('Ctrl Pts',(-0.154607860978349,1.35105447038507,-1.64289183246942));
#8907=CARTESIAN_POINT('Ctrl Pts',(-0.126528390765307,1.33182222741682,-1.64543058688707));
#8908=CARTESIAN_POINT('Ctrl Pts',(-0.0649476351123398,1.30629366210296,
-1.64900971937348));
#8909=CARTESIAN_POINT('Ctrl Pts',(-0.031442345428849,1.3,-1.65));
#8910=CARTESIAN_POINT('Ctrl Pts',(-4.85722573273506E-17,1.3,-1.65));
#8911=CARTESIAN_POINT('',(0.,1.8,1.65));
#8912=CARTESIAN_POINT('',(0.,1.3,1.65));
#8913=CARTESIAN_POINT('Ctrl Pts',(8.32667268468867E-17,1.8,1.65));
#8914=CARTESIAN_POINT('Ctrl Pts',(0.031442345428849,1.8,1.65));
#8915=CARTESIAN_POINT('Ctrl Pts',(0.0649476351123398,1.79370633789704,1.64900971937348));
#8916=CARTESIAN_POINT('Ctrl Pts',(0.126528390765307,1.76817777258318,1.64543058688707));
#8917=CARTESIAN_POINT('Ctrl Pts',(0.154607860978349,1.74894552961493,1.64289183246942));
#8918=CARTESIAN_POINT('Ctrl Pts',(0.198945932189457,1.70460745840382,1.63811406745469));
#8919=CARTESIAN_POINT('Ctrl Pts',(0.218177859368546,1.67652816181843,1.63556247215209));
#8920=CARTESIAN_POINT('Ctrl Pts',(0.243706194926033,1.61494799959182,1.63195388134767));
#8921=CARTESIAN_POINT('Ctrl Pts',(0.25,1.58144291640553,1.63095064303001));
#8922=CARTESIAN_POINT('Ctrl Pts',(0.25,1.51855708359447,1.63095064303001));
#8923=CARTESIAN_POINT('Ctrl Pts',(0.243706194926033,1.48505200040818,1.63195388134767));
#8924=CARTESIAN_POINT('Ctrl Pts',(0.218177859368546,1.42347183818157,1.63556247215209));
#8925=CARTESIAN_POINT('Ctrl Pts',(0.198945932189457,1.39539254159618,1.63811406745469));
#8926=CARTESIAN_POINT('Ctrl Pts',(0.154607860978348,1.35105447038507,1.64289183246942));
#8927=CARTESIAN_POINT('Ctrl Pts',(0.126528390765307,1.33182222741682,1.64543058688707));
#8928=CARTESIAN_POINT('Ctrl Pts',(0.0649476351123397,1.30629366210296,1.64900971937348));
#8929=CARTESIAN_POINT('Ctrl Pts',(0.0314423454288488,1.3,1.65));
#8930=CARTESIAN_POINT('Ctrl Pts',(-1.38777878078145E-17,1.3,1.65));
#8931=CARTESIAN_POINT('',(-0.25,1.55,1.63095064303001));
#8932=CARTESIAN_POINT('Ctrl Pts',(-5.55111512312578E-17,1.3,1.65));
#8933=CARTESIAN_POINT('Ctrl Pts',(-0.031442345428849,1.3,1.65));
#8934=CARTESIAN_POINT('Ctrl Pts',(-0.0649476351123398,1.30629366210296,
1.64900971937348));
#8935=CARTESIAN_POINT('Ctrl Pts',(-0.126528390765307,1.33182222741682,1.64543058688707));
#8936=CARTESIAN_POINT('Ctrl Pts',(-0.154607860978349,1.35105447038507,1.64289183246942));
#8937=CARTESIAN_POINT('Ctrl Pts',(-0.198945932189457,1.39539254159618,1.63811406745469));
#8938=CARTESIAN_POINT('Ctrl Pts',(-0.218177859368546,1.42347183818157,1.63556247215209));
#8939=CARTESIAN_POINT('Ctrl Pts',(-0.243706194926033,1.48505200040818,1.63195388134767));
#8940=CARTESIAN_POINT('Ctrl Pts',(-0.25,1.51855708359447,1.63095064303001));
#8941=CARTESIAN_POINT('Ctrl Pts',(-0.25,1.55,1.63095064303001));
#8942=CARTESIAN_POINT('Ctrl Pts',(-0.25,1.55,1.63095064303001));
#8943=CARTESIAN_POINT('Ctrl Pts',(-0.25,1.58144291640553,1.63095064303001));
#8944=CARTESIAN_POINT('Ctrl Pts',(-0.243706194926033,1.61494799959182,1.63195388134767));
#8945=CARTESIAN_POINT('Ctrl Pts',(-0.218177859368546,1.67652816181843,1.63556247215209));
#8946=CARTESIAN_POINT('Ctrl Pts',(-0.198945932189456,1.70460745840382,1.63811406745469));
#8947=CARTESIAN_POINT('Ctrl Pts',(-0.154607860978348,1.74894552961493,1.64289183246942));
#8948=CARTESIAN_POINT('Ctrl Pts',(-0.126528390765307,1.76817777258318,1.64543058688707));
#8949=CARTESIAN_POINT('Ctrl Pts',(-0.0649476351123396,1.79370633789704,
1.64900971937348));
#8950=CARTESIAN_POINT('Ctrl Pts',(-0.0314423454288488,1.8,1.65));
#8951=CARTESIAN_POINT('Ctrl Pts',(7.63278329429795E-17,1.8,1.65));
#8952=CARTESIAN_POINT('Origin',(0.,1.55,0.));
#8953=CARTESIAN_POINT('',(-0.713525491562421,1.55,0.700629269222037));
#8954=CARTESIAN_POINT('',(0.125,1.55,0.21650635094611));
#8955=CARTESIAN_POINT('Ctrl Pts',(-0.713525491562421,1.55,0.700629269222037));
#8956=CARTESIAN_POINT('Ctrl Pts',(-0.713525491562421,1.5815373526696,0.700629269222037));
#8957=CARTESIAN_POINT('Ctrl Pts',(-0.718163997970498,1.61508042700263,0.695997784676727));
#8958=CARTESIAN_POINT('Ctrl Pts',(-0.73619249062986,1.67663267125761,0.676899590973058));
#8959=CARTESIAN_POINT('Ctrl Pts',(-0.749495710301795,1.70465411363682,0.662390652284073));
#8960=CARTESIAN_POINT('Ctrl Pts',(-0.778498278845144,1.74889618382539,0.628048950774009));
#8961=CARTESIAN_POINT('Ctrl Pts',(-0.796153444118959,1.76811531482682,0.605884303066698));
#8962=CARTESIAN_POINT('Ctrl Pts',(-0.832065554235658,1.79367084275751,0.555538485325663));
#8963=CARTESIAN_POINT('Ctrl Pts',(-0.850258932191534,1.8,0.527308329855002));
#8964=CARTESIAN_POINT('Ctrl Pts',(-0.881791875377343,1.8,0.472691670144998));
#8965=CARTESIAN_POINT('Ctrl Pts',(-0.897143218189782,1.79367084275751,0.442820664919227));
#8966=CARTESIAN_POINT('Ctrl Pts',(-0.92278792026947,1.76811531482682,0.386546956384144));
#8967=CARTESIAN_POINT('Ctrl Pts',(-0.933155485613026,1.74889618382539,0.360174810895352));
#8968=CARTESIAN_POINT('Ctrl Pts',(-0.948394987258249,1.70465411363682,0.31788699900678));
#8969=CARTESIAN_POINT('Ctrl Pts',(-0.954308486908894,1.67663267125761,0.299111603474267));
#8970=CARTESIAN_POINT('Ctrl Pts',(-0.961833761492987,1.61508042700263,0.273949373987484));
#8971=CARTESIAN_POINT('Ctrl Pts',(-0.963525491562421,1.5815373526696,0.267616567329817));
#8972=CARTESIAN_POINT('Ctrl Pts',(-0.963525491562421,1.5184626473304,0.267616567329817));
#8973=CARTESIAN_POINT('Ctrl Pts',(-0.961833761492987,1.48491957299737,0.273949373987484));
#8974=CARTESIAN_POINT('Ctrl Pts',(-0.954308486908894,1.42336732874239,0.299111603474267));
#8975=CARTESIAN_POINT('Ctrl Pts',(-0.948394987258249,1.39534588636318,0.31788699900678));
#8976=CARTESIAN_POINT('Ctrl Pts',(-0.933155485613026,1.35110381617461,0.360174810895352));
#8977=CARTESIAN_POINT('Ctrl Pts',(-0.92278792026947,1.33188468517318,0.386546956384144));
#8978=CARTESIAN_POINT('Ctrl Pts',(-0.897143218189782,1.30632915724249,0.442820664919227));
#8979=CARTESIAN_POINT('Ctrl Pts',(-0.881791875377343,1.3,0.472691670144998));
#8980=CARTESIAN_POINT('Ctrl Pts',(-0.850258932191534,1.3,0.527308329855002));
#8981=CARTESIAN_POINT('Ctrl Pts',(-0.832065554235658,1.30632915724249,0.555538485325663));
#8982=CARTESIAN_POINT('Ctrl Pts',(-0.796153444118959,1.33188468517318,0.605884303066698));
#8983=CARTESIAN_POINT('Ctrl Pts',(-0.778498278845144,1.35110381617461,0.628048950774009));
#8984=CARTESIAN_POINT('Ctrl Pts',(-0.749495710301795,1.39534588636318,0.662390652284073));
#8985=CARTESIAN_POINT('Ctrl Pts',(-0.73619249062986,1.42336732874239,0.676899590973058));
#8986=CARTESIAN_POINT('Ctrl Pts',(-0.718163997970498,1.48491957299737,0.695997784676727));
#8987=CARTESIAN_POINT('Ctrl Pts',(-0.713525491562421,1.5184626473304,0.700629269222037));
#8988=CARTESIAN_POINT('Ctrl Pts',(-0.713525491562421,1.55,0.700629269222037));
#8989=CARTESIAN_POINT('Origin',(0.,1.55,0.));
#8990=CARTESIAN_POINT('',(0.963525491562421,1.55,-0.267616567329817));
#8991=CARTESIAN_POINT('Ctrl Pts',(0.963525491562421,1.55,-0.267616567329817));
#8992=CARTESIAN_POINT('Ctrl Pts',(0.963525491562421,1.5184626473304,-0.267616567329817));
#8993=CARTESIAN_POINT('Ctrl Pts',(0.961833761492987,1.48491957299737,-0.273949373987484));
#8994=CARTESIAN_POINT('Ctrl Pts',(0.954308486908894,1.42336732874239,-0.299111603474267));
#8995=CARTESIAN_POINT('Ctrl Pts',(0.948394987258249,1.39534588636318,-0.31788699900678));
#8996=CARTESIAN_POINT('Ctrl Pts',(0.933155485613026,1.35110381617461,-0.360174810895352));
#8997=CARTESIAN_POINT('Ctrl Pts',(0.92278792026947,1.33188468517318,-0.386546956384144));
#8998=CARTESIAN_POINT('Ctrl Pts',(0.897143218189782,1.30632915724249,-0.442820664919227));
#8999=CARTESIAN_POINT('Ctrl Pts',(0.881791875377343,1.3,-0.472691670144998));
#9000=CARTESIAN_POINT('Ctrl Pts',(0.850258932191534,1.3,-0.527308329855002));
#9001=CARTESIAN_POINT('Ctrl Pts',(0.832065554235658,1.30632915724249,-0.555538485325663));
#9002=CARTESIAN_POINT('Ctrl Pts',(0.796153444118959,1.33188468517318,-0.605884303066698));
#9003=CARTESIAN_POINT('Ctrl Pts',(0.778498278845144,1.35110381617461,-0.628048950774009));
#9004=CARTESIAN_POINT('Ctrl Pts',(0.749495710301795,1.39534588636318,-0.662390652284073));
#9005=CARTESIAN_POINT('Ctrl Pts',(0.73619249062986,1.42336732874239,-0.676899590973058));
#9006=CARTESIAN_POINT('Ctrl Pts',(0.718163997970498,1.48491957299737,-0.695997784676727));
#9007=CARTESIAN_POINT('Ctrl Pts',(0.713525491562421,1.5184626473304,-0.700629269222037));
#9008=CARTESIAN_POINT('Ctrl Pts',(0.713525491562421,1.5815373526696,-0.700629269222037));
#9009=CARTESIAN_POINT('Ctrl Pts',(0.718163997970498,1.61508042700263,-0.695997784676727));
#9010=CARTESIAN_POINT('Ctrl Pts',(0.73619249062986,1.67663267125761,-0.676899590973058));
#9011=CARTESIAN_POINT('Ctrl Pts',(0.749495710301795,1.70465411363682,-0.662390652284073));
#9012=CARTESIAN_POINT('Ctrl Pts',(0.778498278845144,1.74889618382539,-0.628048950774009));
#9013=CARTESIAN_POINT('Ctrl Pts',(0.796153444118959,1.76811531482682,-0.605884303066698));
#9014=CARTESIAN_POINT('Ctrl Pts',(0.832065554235658,1.79367084275751,-0.555538485325663));
#9015=CARTESIAN_POINT('Ctrl Pts',(0.850258932191534,1.8,-0.527308329855002));
#9016=CARTESIAN_POINT('Ctrl Pts',(0.881791875377343,1.8,-0.472691670144998));
#9017=CARTESIAN_POINT('Ctrl Pts',(0.897143218189782,1.79367084275751,-0.442820664919227));
#9018=CARTESIAN_POINT('Ctrl Pts',(0.92278792026947,1.76811531482682,-0.386546956384144));
#9019=CARTESIAN_POINT('Ctrl Pts',(0.933155485613026,1.74889618382539,-0.360174810895352));
#9020=CARTESIAN_POINT('Ctrl Pts',(0.948394987258249,1.70465411363682,-0.31788699900678));
#9021=CARTESIAN_POINT('Ctrl Pts',(0.954308486908894,1.67663267125761,-0.299111603474267));
#9022=CARTESIAN_POINT('Ctrl Pts',(0.961833761492987,1.61508042700263,-0.273949373987484));
#9023=CARTESIAN_POINT('Ctrl Pts',(0.963525491562421,1.5815373526696,-0.267616567329817));
#9024=CARTESIAN_POINT('Ctrl Pts',(0.963525491562421,1.55,-0.267616567329817));
#9025=CARTESIAN_POINT('',(0.125,1.55,0.21650635094611));
#9026=CARTESIAN_POINT('Origin',(0.,1.55,0.));
#9027=CARTESIAN_POINT('',(-0.25,1.55,-0.968245836551854));
#9028=CARTESIAN_POINT('',(-0.25,1.55,0.));
#9029=CARTESIAN_POINT('Ctrl Pts',(-0.25,1.55,-0.968245836551854));
#9030=CARTESIAN_POINT('Ctrl Pts',(-0.25,1.5815373526696,-0.968245836551854));
#9031=CARTESIAN_POINT('Ctrl Pts',(-0.243669763522489,1.61508042700263,-0.969947158664211));
#9032=CARTESIAN_POINT('Ctrl Pts',(-0.218115996279034,1.67663267125761,-0.976011194447325));
#9033=CARTESIAN_POINT('Ctrl Pts',(-0.198899276956455,1.70465411363682,-0.980277651290853));
#9034=CARTESIAN_POINT('Ctrl Pts',(-0.154657206767882,1.74889618382539,-0.988223761669361));
#9035=CARTESIAN_POINT('Ctrl Pts',(-0.126634476150511,1.76811531482682,-0.992431259450842));
#9036=CARTESIAN_POINT('Ctrl Pts',(-0.0650776639541238,1.79367084275751,
-0.99835915024489));
#9037=CARTESIAN_POINT('Ctrl Pts',(-0.0315329431858092,1.8,-1.));
#9038=CARTESIAN_POINT('Ctrl Pts',(0.0315329431858092,1.8,-1.));
#9039=CARTESIAN_POINT('Ctrl Pts',(0.0650776639541238,1.79367084275751,-0.99835915024489));
#9040=CARTESIAN_POINT('Ctrl Pts',(0.126634476150511,1.76811531482682,-0.992431259450842));
#9041=CARTESIAN_POINT('Ctrl Pts',(0.154657206767882,1.74889618382539,-0.988223761669361));
#9042=CARTESIAN_POINT('Ctrl Pts',(0.198899276956455,1.70465411363682,-0.980277651290853));
#9043=CARTESIAN_POINT('Ctrl Pts',(0.218115996279034,1.67663267125761,-0.976011194447325));
#9044=CARTESIAN_POINT('Ctrl Pts',(0.243669763522488,1.61508042700263,-0.969947158664211));
#9045=CARTESIAN_POINT('Ctrl Pts',(0.25,1.5815373526696,-0.968245836551854));
#9046=CARTESIAN_POINT('Ctrl Pts',(0.25,1.5184626473304,-0.968245836551854));
#9047=CARTESIAN_POINT('Ctrl Pts',(0.243669763522488,1.48491957299737,-0.969947158664211));
#9048=CARTESIAN_POINT('Ctrl Pts',(0.218115996279034,1.42336732874239,-0.976011194447325));
#9049=CARTESIAN_POINT('Ctrl Pts',(0.198899276956455,1.39534588636318,-0.980277651290853));
#9050=CARTESIAN_POINT('Ctrl Pts',(0.154657206767882,1.35110381617461,-0.988223761669361));
#9051=CARTESIAN_POINT('Ctrl Pts',(0.126634476150511,1.33188468517318,-0.992431259450842));
#9052=CARTESIAN_POINT('Ctrl Pts',(0.0650776639541239,1.30632915724249,-0.99835915024489));
#9053=CARTESIAN_POINT('Ctrl Pts',(0.0315329431858092,1.3,-1.));
#9054=CARTESIAN_POINT('Ctrl Pts',(-0.0315329431858092,1.3,-1.));
#9055=CARTESIAN_POINT('Ctrl Pts',(-0.0650776639541239,1.30632915724249,
-0.99835915024489));
#9056=CARTESIAN_POINT('Ctrl Pts',(-0.126634476150511,1.33188468517318,-0.992431259450842));
#9057=CARTESIAN_POINT('Ctrl Pts',(-0.154657206767882,1.35110381617461,-0.988223761669361));
#9058=CARTESIAN_POINT('Ctrl Pts',(-0.198899276956455,1.39534588636318,-0.980277651290853));
#9059=CARTESIAN_POINT('Ctrl Pts',(-0.218115996279034,1.42336732874239,-0.976011194447325));
#9060=CARTESIAN_POINT('Ctrl Pts',(-0.243669763522489,1.48491957299737,-0.969947158664211));
#9061=CARTESIAN_POINT('Ctrl Pts',(-0.25,1.5184626473304,-0.968245836551854));
#9062=CARTESIAN_POINT('Ctrl Pts',(-0.25,1.55,-0.968245836551854));
#9063=CARTESIAN_POINT('Origin',(0.,1.55,0.));
#9064=CARTESIAN_POINT('',(-0.25,1.55,0.968245836551854));
#9065=CARTESIAN_POINT('Ctrl Pts',(-0.25,1.55,0.968245836551854));
#9066=CARTESIAN_POINT('Ctrl Pts',(-0.25,1.5184626473304,0.968245836551854));
#9067=CARTESIAN_POINT('Ctrl Pts',(-0.243669763522489,1.48491957299737,0.969947158664211));
#9068=CARTESIAN_POINT('Ctrl Pts',(-0.218115996279034,1.42336732874239,0.976011194447325));
#9069=CARTESIAN_POINT('Ctrl Pts',(-0.198899276956455,1.39534588636318,0.980277651290853));
#9070=CARTESIAN_POINT('Ctrl Pts',(-0.154657206767882,1.35110381617461,0.988223761669361));
#9071=CARTESIAN_POINT('Ctrl Pts',(-0.126634476150511,1.33188468517318,0.992431259450842));
#9072=CARTESIAN_POINT('Ctrl Pts',(-0.065077663954124,1.30632915724249,0.99835915024489));
#9073=CARTESIAN_POINT('Ctrl Pts',(-0.0315329431858092,1.3,1.));
#9074=CARTESIAN_POINT('Ctrl Pts',(0.0315329431858092,1.3,1.));
#9075=CARTESIAN_POINT('Ctrl Pts',(0.065077663954124,1.30632915724249,0.99835915024489));
#9076=CARTESIAN_POINT('Ctrl Pts',(0.126634476150511,1.33188468517318,0.992431259450842));
#9077=CARTESIAN_POINT('Ctrl Pts',(0.154657206767882,1.35110381617461,0.988223761669361));
#9078=CARTESIAN_POINT('Ctrl Pts',(0.198899276956455,1.39534588636318,0.980277651290853));
#9079=CARTESIAN_POINT('Ctrl Pts',(0.218115996279034,1.42336732874239,0.976011194447325));
#9080=CARTESIAN_POINT('Ctrl Pts',(0.243669763522488,1.48491957299737,0.969947158664211));
#9081=CARTESIAN_POINT('Ctrl Pts',(0.25,1.5184626473304,0.968245836551854));
#9082=CARTESIAN_POINT('Ctrl Pts',(0.25,1.5815373526696,0.968245836551854));
#9083=CARTESIAN_POINT('Ctrl Pts',(0.243669763522488,1.61508042700263,0.969947158664211));
#9084=CARTESIAN_POINT('Ctrl Pts',(0.218115996279034,1.67663267125761,0.976011194447325));
#9085=CARTESIAN_POINT('Ctrl Pts',(0.198899276956455,1.70465411363682,0.980277651290853));
#9086=CARTESIAN_POINT('Ctrl Pts',(0.154657206767882,1.74889618382539,0.988223761669361));
#9087=CARTESIAN_POINT('Ctrl Pts',(0.126634476150511,1.76811531482682,0.992431259450842));
#9088=CARTESIAN_POINT('Ctrl Pts',(0.0650776639541239,1.79367084275751,0.99835915024489));
#9089=CARTESIAN_POINT('Ctrl Pts',(0.0315329431858092,1.8,1.));
#9090=CARTESIAN_POINT('Ctrl Pts',(-0.0315329431858092,1.8,1.));
#9091=CARTESIAN_POINT('Ctrl Pts',(-0.0650776639541239,1.79367084275751,
0.99835915024489));
#9092=CARTESIAN_POINT('Ctrl Pts',(-0.126634476150511,1.76811531482682,0.992431259450842));
#9093=CARTESIAN_POINT('Ctrl Pts',(-0.154657206767882,1.74889618382539,0.988223761669361));
#9094=CARTESIAN_POINT('Ctrl Pts',(-0.198899276956455,1.70465411363682,0.980277651290853));
#9095=CARTESIAN_POINT('Ctrl Pts',(-0.218115996279034,1.67663267125761,0.976011194447325));
#9096=CARTESIAN_POINT('Ctrl Pts',(-0.243669763522489,1.61508042700263,0.969947158664211));
#9097=CARTESIAN_POINT('Ctrl Pts',(-0.25,1.5815373526696,0.968245836551854));
#9098=CARTESIAN_POINT('Ctrl Pts',(-0.25,1.55,0.968245836551854));
#9099=CARTESIAN_POINT('',(-0.25,1.55,0.));
#9100=CARTESIAN_POINT('Origin',(1.65,2.25,0.));
#9101=CARTESIAN_POINT('',(-1.,2.25,-1.22464679914735E-16));
#9102=CARTESIAN_POINT('Origin',(0.,2.25,0.));
#9103=CARTESIAN_POINT('Origin',(1.75,0.85,0.));
#9104=CARTESIAN_POINT('',(-1.75,0.85,-2.14313189850787E-16));
#9105=CARTESIAN_POINT('Origin',(0.,0.85,0.));
#9106=CARTESIAN_POINT('Origin',(0.,0.,0.));
#9107=CARTESIAN_POINT('',(-1.75,-0.85,-2.14313189850787E-16));
#9108=CARTESIAN_POINT('Origin',(0.,-0.85,0.));
#9109=CARTESIAN_POINT('',(-1.75,0.,-2.14313189850787E-16));
#9110=CARTESIAN_POINT('Origin',(1.,-0.85,0.));
#9111=CARTESIAN_POINT('',(-1.,-0.85,-1.22464679914735E-16));
#9112=CARTESIAN_POINT('Origin',(0.,-0.85,0.));
#9113=CARTESIAN_POINT('Origin',(0.,0.7,0.));
#9114=CARTESIAN_POINT('',(-1.,0.7,-1.22464679914735E-16));
#9115=CARTESIAN_POINT('',(0.,0.,0.));
#9116=CARTESIAN_POINT('',(0.,0.,0.));
#9117=CARTESIAN_POINT('',(0.,0.,0.));
#9118=CARTESIAN_POINT('Origin',(0.,0.,0.));
#9119=CARTESIAN_POINT('',(-0.42,0.16,5.14351655641888E-17));
#9120=CARTESIAN_POINT('Origin',(0.,0.16,0.));
#9121=CARTESIAN_POINT('',(-0.42,0.,5.14351655641888E-17));
#9122=CARTESIAN_POINT('',(-0.42,0.,5.14351655641888E-17));
#9123=CARTESIAN_POINT('Origin',(0.,0.,0.));
#9124=CARTESIAN_POINT('Origin',(0.,0.,0.));
#9125=CARTESIAN_POINT('',(-0.8,0.16,9.79717439317883E-17));
#9126=CARTESIAN_POINT('Origin',(0.,0.16,0.));
#9127=CARTESIAN_POINT('',(-0.8,0.,9.79717439317883E-17));
#9128=CARTESIAN_POINT('',(-0.8,0.,9.79717439317883E-17));
#9129=CARTESIAN_POINT('Origin',(0.,0.,0.));
#9130=CARTESIAN_POINT('Origin',(0.,0.16,0.));
#9131=CARTESIAN_POINT('Origin',(0.,0.,0.));
#9132=CARTESIAN_POINT('',(0.,0.,0.));
#9133=CARTESIAN_POINT('Origin',(0.173205080756888,-0.8,-0.3));
#9134=CARTESIAN_POINT('',(0.346410161513775,-0.8,0.));
#9135=CARTESIAN_POINT('',(0.173205080756888,-0.8,-0.3));
#9136=CARTESIAN_POINT('',(0.346410161513775,-0.8,0.));
#9137=CARTESIAN_POINT('',(0.173205080756888,-1.28,-0.3));
#9138=CARTESIAN_POINT('',(0.173205080756888,-0.8,-0.3));
#9139=CARTESIAN_POINT('',(0.346410161513775,-1.28,0.));
#9140=CARTESIAN_POINT('',(0.346410161513775,-1.28,0.));
#9141=CARTESIAN_POINT('',(0.346410161513775,-0.8,0.));
#9142=CARTESIAN_POINT('Origin',(-0.173205080756888,-0.8,-0.3));
#9143=CARTESIAN_POINT('',(-0.173205080756888,-0.8,-0.3));
#9144=CARTESIAN_POINT('',(0.173205080756888,-0.8,-0.3));
#9145=CARTESIAN_POINT('',(-0.173205080756888,-1.28,-0.3));
#9146=CARTESIAN_POINT('',(-0.173205080756888,-0.8,-0.3));
#9147=CARTESIAN_POINT('',(0.173205080756888,-1.28,-0.3));
#9148=CARTESIAN_POINT('Origin',(-0.346410161513775,-0.8,-5.55111512312578E-17));
#9149=CARTESIAN_POINT('',(-0.346410161513775,-0.8,-4.24230095489963E-17));
#9150=CARTESIAN_POINT('',(-0.173205080756888,-0.8,-0.3));
#9151=CARTESIAN_POINT('',(-0.346410161513775,-1.28,-5.55111512312578E-17));
#9152=CARTESIAN_POINT('',(-0.346410161513775,-0.8,-4.24230095489963E-17));
#9153=CARTESIAN_POINT('',(-0.173205080756888,-1.28,-0.3));
#9154=CARTESIAN_POINT('Origin',(-0.173205080756888,-0.8,0.3));
#9155=CARTESIAN_POINT('',(-0.173205080756888,-0.8,0.3));
#9156=CARTESIAN_POINT('',(-0.346410161513775,-0.8,-4.24230095489963E-17));
#9157=CARTESIAN_POINT('',(-0.173205080756888,-1.28,0.3));
#9158=CARTESIAN_POINT('',(-0.173205080756888,-0.8,0.3));
#9159=CARTESIAN_POINT('',(-0.346410161513775,-1.28,-4.24230095489963E-17));
#9160=CARTESIAN_POINT('Origin',(0.173205080756888,-0.8,0.3));
#9161=CARTESIAN_POINT('',(0.173205080756888,-0.8,0.3));
#9162=CARTESIAN_POINT('',(-0.173205080756888,-0.8,0.3));
#9163=CARTESIAN_POINT('',(0.173205080756888,-1.28,0.3));
#9164=CARTESIAN_POINT('',(0.173205080756888,-0.8,0.3));
#9165=CARTESIAN_POINT('',(-0.173205080756888,-1.28,0.3));
#9166=CARTESIAN_POINT('Origin',(0.346410161513775,-0.8,0.));
#9167=CARTESIAN_POINT('',(0.173205080756888,-0.8,0.3));
#9168=CARTESIAN_POINT('',(0.173205080756888,-1.28,0.3));
#9169=CARTESIAN_POINT('Origin',(0.,-0.8,-5.55111512312578E-17));
#9170=CARTESIAN_POINT('Origin',(0.,-1.28,-5.55111512312578E-17));
#9171=CARTESIAN_POINT('Origin',(0.,-2.5,0.));
#9172=CARTESIAN_POINT('',(-0.3933,-2.5,4.81653586104654E-17));
#9173=CARTESIAN_POINT('Origin',(0.,-2.5,0.));
#9174=CARTESIAN_POINT('Origin',(0.6,0.8,0.));
#9175=CARTESIAN_POINT('',(-0.6,0.8,-7.34788079488412E-17));
#9176=CARTESIAN_POINT('Origin',(0.,0.8,0.));
#9177=CARTESIAN_POINT('Origin',(0.,0.775,0.));
#9178=CARTESIAN_POINT('',(-0.65,0.75,-7.9602041944578E-17));
#9179=CARTESIAN_POINT('Origin',(0.,0.75,0.));
#9180=CARTESIAN_POINT('',(-0.625,0.775,-7.65404249467096E-17));
#9181=CARTESIAN_POINT('Origin',(0.,0.39,0.));
#9182=CARTESIAN_POINT('',(-0.65,0.0299999999999998,-7.9602041944578E-17));
#9183=CARTESIAN_POINT('Origin',(0.,0.0299999999999998,0.));
#9184=CARTESIAN_POINT('',(-0.65,0.39,-7.9602041944578E-17));
#9185=CARTESIAN_POINT('Origin',(0.,0.0150000000000001,0.));
#9186=CARTESIAN_POINT('',(-0.62,5.89805981832114E-17,-7.59281015471359E-17));
#9187=CARTESIAN_POINT('Origin',(0.,0.,0.));
#9188=CARTESIAN_POINT('',(-0.635,0.0150000000000001,-7.77650717458569E-17));
#9189=CARTESIAN_POINT('Origin',(0.42,0.,0.));
#9190=CARTESIAN_POINT('',(-0.42,-3.46944695195361E-18,-5.14351655641888E-17));
#9191=CARTESIAN_POINT('Origin',(0.,0.,0.));
#9192=CARTESIAN_POINT('Origin',(0.,-0.02,0.));
#9193=CARTESIAN_POINT('',(-0.3933,-0.0534000000000001,4.81653586104654E-17));
#9194=CARTESIAN_POINT('Origin',(0.,-0.0534000000000001,0.));
#9195=CARTESIAN_POINT('',(-0.41,-0.02,-5.02105187650415E-17));
#9196=CARTESIAN_POINT('Origin',(0.,-1.48,0.));
#9197=CARTESIAN_POINT('',(-0.3933,-1.48,-4.81653586104654E-17));
#9198=CARTESIAN_POINT('',(0.,0.,0.));
#9199=CARTESIAN_POINT('',(0.,0.,0.));
#9200=CARTESIAN_POINT('',(0.,0.,0.));
#9201=CARTESIAN_POINT('',(0.,0.,0.));
#9202=CARTESIAN_POINT('',(0.,0.,0.));
#9203=CARTESIAN_POINT('',(0.,0.,0.));
#9204=CARTESIAN_POINT('',(0.,0.,0.));
#9205=CARTESIAN_POINT('',(0.,0.,4.53));
#9206=CARTESIAN_POINT('',(-4.75,0.,2.4));
#9207=CARTESIAN_POINT('',(-4.75,0.,2.56));
#9208=CARTESIAN_POINT('',(4.75,0.,2.4));
#9209=CARTESIAN_POINT('',(4.75,0.,2.56));
#9210=CARTESIAN_POINT('',(0.,20.,4.53));
#9211=CARTESIAN_POINT('',(-4.75,20.,2.4));
#9212=CARTESIAN_POINT('',(-4.75,20.,2.56));
#9213=CARTESIAN_POINT('',(4.75,20.,2.4));
#9214=CARTESIAN_POINT('',(4.75,20.,2.56));
#9215=CARTESIAN_POINT('',(0.,0.,0.));
#9216=CARTESIAN_POINT('',(0.,0.,0.));
#9217=CARTESIAN_POINT('Origin',(-0.3,9.2,3.43));
#9218=CARTESIAN_POINT('',(-0.3,11.2,3.57606079858305));
#9219=CARTESIAN_POINT('',(-0.3,9.2,3.57606079858305));
#9220=CARTESIAN_POINT('',(-0.3,-2.5,3.57606079858305));
#9221=CARTESIAN_POINT('',(-0.3,11.2,3.88));
#9222=CARTESIAN_POINT('',(-0.3,11.2,3.88));
#9223=CARTESIAN_POINT('',(-0.3,9.2,3.88));
#9224=CARTESIAN_POINT('',(-0.3,9.2,3.88));
#9225=CARTESIAN_POINT('',(-0.3,9.2,3.88));
#9226=CARTESIAN_POINT('Origin',(0.,9.2,3.655));
#9227=CARTESIAN_POINT('',(0.3,9.2,3.57606079858305));
#9228=CARTESIAN_POINT('Origin',(0.,9.2,4.53));
#9229=CARTESIAN_POINT('',(0.3,9.2,3.88));
#9230=CARTESIAN_POINT('',(0.3,9.2,3.88));
#9231=CARTESIAN_POINT('',(0.3,9.2,3.43));
#9232=CARTESIAN_POINT('Origin',(0.3,9.2,3.88));
#9233=CARTESIAN_POINT('',(0.3,11.2,3.57606079858305));
#9234=CARTESIAN_POINT('',(0.3,-2.5,3.57606079858305));
#9235=CARTESIAN_POINT('',(0.3,11.2,3.88));
#9236=CARTESIAN_POINT('',(0.3,9.2,3.88));
#9237=CARTESIAN_POINT('',(0.3,11.2,3.43));
#9238=CARTESIAN_POINT('Origin',(-0.3,9.2,3.88));
#9239=CARTESIAN_POINT('',(0.3,11.2,3.88));
#9240=CARTESIAN_POINT('Origin',(0.,11.2,3.655));
#9241=CARTESIAN_POINT('Origin',(0.,11.2,4.53));
#9242=CARTESIAN_POINT('Origin',(0.,25.,4.53));
#9243=CARTESIAN_POINT('',(-0.21,25.,4.53));
#9244=CARTESIAN_POINT('Origin',(0.,25.,4.53));
#9245=CARTESIAN_POINT('',(-0.21,27.,4.53));
#9246=CARTESIAN_POINT('',(-0.21,25.,4.53));
#9247=CARTESIAN_POINT('Origin',(0.,27.,4.53));
#9248=CARTESIAN_POINT('Origin',(0.,25.,4.53));
#9249=CARTESIAN_POINT('Origin',(0.,-5.6,4.53));
#9250=CARTESIAN_POINT('',(-0.21,-5.5,4.53));
#9251=CARTESIAN_POINT('Origin',(0.,-5.5,4.53));
#9252=CARTESIAN_POINT('',(-0.21,-3.5,4.53));
#9253=CARTESIAN_POINT('',(-0.21,-5.6,4.53));
#9254=CARTESIAN_POINT('Origin',(0.,-3.5,4.53));
#9255=CARTESIAN_POINT('Origin',(0.,-3.5,4.53));
#9256=CARTESIAN_POINT('Origin',(-0.2,24.15,3.83));
#9257=CARTESIAN_POINT('',(-0.2,25.6,3.96431457505076));
#9258=CARTESIAN_POINT('',(-0.2,24.15,3.96431457505076));
#9259=CARTESIAN_POINT('',(-0.2,24.,3.96431457505076));
#9260=CARTESIAN_POINT('',(-0.2,25.6,4.18));
#9261=CARTESIAN_POINT('',(-0.2,25.6,4.18));
#9262=CARTESIAN_POINT('',(-0.2,24.15,4.18));
#9263=CARTESIAN_POINT('',(-0.2,24.15,4.18));
#9264=CARTESIAN_POINT('',(-0.2,24.15,4.18));
#9265=CARTESIAN_POINT('Origin',(0.,24.15,4.005));
#9266=CARTESIAN_POINT('',(0.2,24.15,3.96431457505076));
#9267=CARTESIAN_POINT('Origin',(0.,24.15,4.53));
#9268=CARTESIAN_POINT('',(0.2,24.15,4.18));
#9269=CARTESIAN_POINT('',(0.2,24.15,4.18));
#9270=CARTESIAN_POINT('',(0.2,24.15,3.83));
#9271=CARTESIAN_POINT('Origin',(0.2,24.15,4.18));
#9272=CARTESIAN_POINT('',(0.2,25.6,3.96431457505076));
#9273=CARTESIAN_POINT('',(0.2,24.,3.96431457505076));
#9274=CARTESIAN_POINT('',(0.2,25.6,4.18));
#9275=CARTESIAN_POINT('',(0.2,24.15,4.18));
#9276=CARTESIAN_POINT('',(0.2,25.6,3.83));
#9277=CARTESIAN_POINT('Origin',(-0.2,24.15,4.18));
#9278=CARTESIAN_POINT('',(0.2,25.6,4.18));
#9279=CARTESIAN_POINT('Origin',(0.,25.6,4.005));
#9280=CARTESIAN_POINT('Origin',(0.,25.6,4.53));
#9281=CARTESIAN_POINT('Origin',(-0.2,-5.05,3.83));
#9282=CARTESIAN_POINT('',(-0.2,-3.6,3.96431457505076));
#9283=CARTESIAN_POINT('',(-0.2,-5.05,3.96431457505076));
#9284=CARTESIAN_POINT('',(-0.2,-5.5,3.96431457505076));
#9285=CARTESIAN_POINT('',(-0.2,-3.6,4.18));
#9286=CARTESIAN_POINT('',(-0.2,-3.6,4.18));
#9287=CARTESIAN_POINT('',(-0.2,-5.05,4.18));
#9288=CARTESIAN_POINT('',(-0.2,-5.05,4.18));
#9289=CARTESIAN_POINT('',(-0.2,-5.05,4.18));
#9290=CARTESIAN_POINT('Origin',(0.,-5.05,4.005));
#9291=CARTESIAN_POINT('',(0.2,-5.05,3.96431457505076));
#9292=CARTESIAN_POINT('Origin',(0.,-5.05,4.53));
#9293=CARTESIAN_POINT('',(0.2,-5.05,4.18));
#9294=CARTESIAN_POINT('',(0.2,-5.05,4.18));
#9295=CARTESIAN_POINT('',(0.2,-5.05,3.83));
#9296=CARTESIAN_POINT('Origin',(0.2,-5.05,4.18));
#9297=CARTESIAN_POINT('',(0.2,-3.6,3.96431457505076));
#9298=CARTESIAN_POINT('',(0.2,-5.5,3.96431457505076));
#9299=CARTESIAN_POINT('',(0.2,-3.6,4.18));
#9300=CARTESIAN_POINT('',(0.2,-5.05,4.18));
#9301=CARTESIAN_POINT('',(0.2,-3.6,3.83));
#9302=CARTESIAN_POINT('Origin',(-0.2,-5.05,4.18));
#9303=CARTESIAN_POINT('',(0.2,-3.6,4.18));
#9304=CARTESIAN_POINT('Origin',(0.,-3.6,4.005));
#9305=CARTESIAN_POINT('Origin',(0.,-3.6,4.53));
#9306=CARTESIAN_POINT('Origin',(0.,24.,4.53));
#9307=CARTESIAN_POINT('',(-0.6,27.,4.53));
#9308=CARTESIAN_POINT('Origin',(0.,27.,4.53));
#9309=CARTESIAN_POINT('',(-0.6,24.,4.53));
#9310=CARTESIAN_POINT('',(-0.6,24.,4.53));
#9311=CARTESIAN_POINT('Origin',(0.,24.,4.53));
#9312=CARTESIAN_POINT('Origin',(0.,27.,4.53));
#9313=CARTESIAN_POINT('Origin',(0.,-5.5,4.53));
#9314=CARTESIAN_POINT('',(-0.6,-2.5,4.53));
#9315=CARTESIAN_POINT('Origin',(0.,-2.5,4.53));
#9316=CARTESIAN_POINT('',(-0.6,-5.5,4.53));
#9317=CARTESIAN_POINT('',(-0.6,-5.5,4.53));
#9318=CARTESIAN_POINT('Origin',(0.,-5.5,4.53));
#9319=CARTESIAN_POINT('Origin',(0.,-5.5,4.53));
#9320=CARTESIAN_POINT('Origin',(0.,-2.5,4.53));
#9321=CARTESIAN_POINT('',(-1.,24.,4.53));
#9322=CARTESIAN_POINT('Origin',(0.,24.,4.53));
#9323=CARTESIAN_POINT('',(-1.,-2.5,4.53));
#9324=CARTESIAN_POINT('',(-1.,-2.5,4.53));
#9325=CARTESIAN_POINT('Origin',(0.,-2.5,4.53));
#9326=CARTESIAN_POINT('Origin',(0.,24.,4.53));
#9327=CARTESIAN_POINT('Origin',(0.,-2.5,4.53));
#9328=CARTESIAN_POINT('',(0.,0.,0.));
#9329=CARTESIAN_POINT('Origin',(0.,-3.45,4.53));
#9330=CARTESIAN_POINT('',(-0.605,-2.5,4.53));
#9331=CARTESIAN_POINT('Origin',(0.,-2.5,4.53));
#9332=CARTESIAN_POINT('',(-0.605,-3.45,4.53));
#9333=CARTESIAN_POINT('',(-0.605,-3.45,4.53));
#9334=CARTESIAN_POINT('Origin',(0.,-3.45,4.53));
#9335=CARTESIAN_POINT('Origin',(0.,-3.45,4.53));
#9336=CARTESIAN_POINT('',(-0.9,-2.5,4.53));
#9337=CARTESIAN_POINT('Origin',(0.,-2.5,4.53));
#9338=CARTESIAN_POINT('',(-0.9,-3.45,4.53));
#9339=CARTESIAN_POINT('',(-0.9,-3.45,4.53));
#9340=CARTESIAN_POINT('Origin',(0.,-3.45,4.53));
#9341=CARTESIAN_POINT('Origin',(0.,-2.5,4.53));
#9342=CARTESIAN_POINT('Origin',(0.,-3.45,4.53));
#9343=CARTESIAN_POINT('',(0.,0.,0.));
#9344=CARTESIAN_POINT('Origin',(0.,25.75,4.53));
#9345=CARTESIAN_POINT('',(-0.605,27.,4.53));
#9346=CARTESIAN_POINT('Origin',(0.,27.,4.53));
#9347=CARTESIAN_POINT('',(-0.605,25.75,4.53));
#9348=CARTESIAN_POINT('',(-0.605,25.75,4.53));
#9349=CARTESIAN_POINT('Origin',(0.,25.75,4.53));
#9350=CARTESIAN_POINT('Origin',(0.,25.75,4.53));
#9351=CARTESIAN_POINT('',(-0.9,27.,4.53));
#9352=CARTESIAN_POINT('Origin',(0.,27.,4.53));
#9353=CARTESIAN_POINT('',(-0.9,25.75,4.53));
#9354=CARTESIAN_POINT('',(-0.9,25.75,4.53));
#9355=CARTESIAN_POINT('Origin',(0.,25.75,4.53));
#9356=CARTESIAN_POINT('Origin',(0.,27.,4.53));
#9357=CARTESIAN_POINT('Origin',(0.,25.75,4.53));
#9358=CARTESIAN_POINT('',(0.,0.,0.));
#9359=CARTESIAN_POINT('Origin',(0.,-5.5,4.53));
#9360=CARTESIAN_POINT('',(-0.605,-5.2,4.53));
#9361=CARTESIAN_POINT('Origin',(0.,-5.2,4.53));
#9362=CARTESIAN_POINT('',(-0.605,-5.5,4.53));
#9363=CARTESIAN_POINT('',(-0.605,-5.5,4.53));
#9364=CARTESIAN_POINT('Origin',(0.,-5.5,4.53));
#9365=CARTESIAN_POINT('Origin',(0.,-5.5,4.53));
#9366=CARTESIAN_POINT('',(-0.9,-5.2,4.53));
#9367=CARTESIAN_POINT('Origin',(0.,-5.2,4.53));
#9368=CARTESIAN_POINT('',(-0.9,-5.5,4.53));
#9369=CARTESIAN_POINT('',(-0.9,-5.5,4.53));
#9370=CARTESIAN_POINT('Origin',(0.,-5.5,4.53));
#9371=CARTESIAN_POINT('Origin',(0.,-5.2,4.53));
#9372=CARTESIAN_POINT('Origin',(0.,-5.5,4.53));
#9373=CARTESIAN_POINT('',(0.,0.,0.));
#9374=CARTESIAN_POINT('Origin',(0.,-5.7,4.53));
#9375=CARTESIAN_POINT('',(-0.275,-5.5,4.53));
#9376=CARTESIAN_POINT('Origin',(0.,-5.5,4.53));
#9377=CARTESIAN_POINT('',(-0.275,-5.7,4.53));
#9378=CARTESIAN_POINT('',(-0.275,-5.7,4.53));
#9379=CARTESIAN_POINT('Origin',(0.,-5.7,4.53));
#9380=CARTESIAN_POINT('Origin',(0.,-5.7,4.53));
#9381=CARTESIAN_POINT('',(-1.,-5.5,4.53));
#9382=CARTESIAN_POINT('Origin',(0.,-5.5,4.53));
#9383=CARTESIAN_POINT('',(-1.,-5.7,4.53));
#9384=CARTESIAN_POINT('',(-1.,-5.7,4.53));
#9385=CARTESIAN_POINT('Origin',(0.,-5.7,4.53));
#9386=CARTESIAN_POINT('Origin',(0.,-5.5,4.53));
#9387=CARTESIAN_POINT('Origin',(0.,-5.7,4.53));
#9388=CARTESIAN_POINT('',(0.,0.,0.));
#9389=CARTESIAN_POINT('Origin',(0.,27.,4.53));
#9390=CARTESIAN_POINT('',(-0.275,27.2,4.53));
#9391=CARTESIAN_POINT('Origin',(0.,27.2,4.53));
#9392=CARTESIAN_POINT('',(-0.275,27.,4.53));
#9393=CARTESIAN_POINT('',(-0.275,27.,4.53));
#9394=CARTESIAN_POINT('Origin',(0.,27.,4.53));
#9395=CARTESIAN_POINT('Origin',(0.,27.,4.53));
#9396=CARTESIAN_POINT('',(-1.,27.2,4.53));
#9397=CARTESIAN_POINT('Origin',(0.,27.2,4.53));
#9398=CARTESIAN_POINT('',(-1.,27.,4.53));
#9399=CARTESIAN_POINT('',(-1.,27.,4.53));
#9400=CARTESIAN_POINT('Origin',(0.,27.,4.53));
#9401=CARTESIAN_POINT('Origin',(0.,27.2,4.53));
#9402=CARTESIAN_POINT('Origin',(0.,27.,4.53));
#9403=CARTESIAN_POINT('',(0.,0.,0.));
#9404=CARTESIAN_POINT('Origin',(0.,10.2,5.52));
#9405=CARTESIAN_POINT('',(0.141067359796651,10.044436508139,5.52));
#9406=CARTESIAN_POINT('',(0.141067359796651,10.355563491861,5.52));
#9407=CARTESIAN_POINT('',(0.141067359796651,9.,5.52));
#9408=CARTESIAN_POINT('Origin',(0.,10.2,5.52));
#9409=CARTESIAN_POINT('Origin',(0.,10.2,5.52));
#9410=CARTESIAN_POINT('',(-0.141067359796651,10.044436508139,5.52));
#9411=CARTESIAN_POINT('Ctrl Pts',(-0.141067359796651,10.044436508139,5.52));
#9412=CARTESIAN_POINT('Ctrl Pts',(-0.123818356698219,10.0287948476368,5.52245784982447));
#9413=CARTESIAN_POINT('Ctrl Pts',(-0.102998643109696,10.015375956669,5.52493819304946));
#9414=CARTESIAN_POINT('Ctrl Pts',(-0.0546141143983528,9.99530253627557,
5.52884449237241));
#9415=CARTESIAN_POINT('Ctrl Pts',(-0.0264520736824499,9.99,5.53));
#9416=CARTESIAN_POINT('Ctrl Pts',(0.0264520736824499,9.99,5.53));
#9417=CARTESIAN_POINT('Ctrl Pts',(0.0546141143983523,9.99530253627557,5.52884449237241));
#9418=CARTESIAN_POINT('Ctrl Pts',(0.102998643109696,10.015375956669,5.52493819304946));
#9419=CARTESIAN_POINT('Ctrl Pts',(0.123818356698219,10.0287948476368,5.52245784982447));
#9420=CARTESIAN_POINT('Ctrl Pts',(0.141067359796652,10.044436508139,5.52));
#9421=CARTESIAN_POINT('',(-0.21,10.2,5.52));
#9422=CARTESIAN_POINT('Origin',(0.,10.2,5.52));
#9423=CARTESIAN_POINT('',(-0.21,10.2,6.51894444366855));
#9424=CARTESIAN_POINT('',(-0.21,10.2,5.52));
#9425=CARTESIAN_POINT('',(0.21,10.2,6.51894444366855));
#9426=CARTESIAN_POINT('Ctrl Pts',(0.21,10.2,6.51894444366855));
#9427=CARTESIAN_POINT('Ctrl Pts',(0.21,10.1736109916407,6.51894444366855));
#9428=CARTESIAN_POINT('Ctrl Pts',(0.204722164681422,10.1454764062218,6.51952376620524));
#9429=CARTESIAN_POINT('Ctrl Pts',(0.183284867450471,10.0937425531788,6.52161307432363));
#9430=CARTESIAN_POINT('Ctrl Pts',(0.167126466290584,10.0701416181922,6.52309254589373));
#9431=CARTESIAN_POINT('Ctrl Pts',(0.129858458976496,10.0328736108781,6.52586721250997));
#9432=CARTESIAN_POINT('Ctrl Pts',(0.106257490219277,10.0167151494345,6.527343117591));
#9433=CARTESIAN_POINT('Ctrl Pts',(0.0545235237847863,9.99527780741314,6.52942425936951));
#9434=CARTESIAN_POINT('Ctrl Pts',(0.0263888990751172,9.99,6.53));
#9435=CARTESIAN_POINT('Ctrl Pts',(-0.0263888990751171,9.99,6.53));
#9436=CARTESIAN_POINT('Ctrl Pts',(-0.0545235237847855,9.99527780741314,
6.52942425936951));
#9437=CARTESIAN_POINT('Ctrl Pts',(-0.106257490219277,10.0167151494345,6.527343117591));
#9438=CARTESIAN_POINT('Ctrl Pts',(-0.129858458976496,10.0328736108781,6.52586721250997));
#9439=CARTESIAN_POINT('Ctrl Pts',(-0.167126466290584,10.0701416181922,6.52309254589373));
#9440=CARTESIAN_POINT('Ctrl Pts',(-0.183284867450472,10.0937425531788,6.52161307432363));
#9441=CARTESIAN_POINT('Ctrl Pts',(-0.204722164681422,10.1454764062218,6.51952376620524));
#9442=CARTESIAN_POINT('Ctrl Pts',(-0.21,10.1736109916407,6.51894444366855));
#9443=CARTESIAN_POINT('Ctrl Pts',(-0.21,10.2,6.51894444366855));
#9444=CARTESIAN_POINT('Ctrl Pts',(-0.21,10.2,6.51894444366855));
#9445=CARTESIAN_POINT('Ctrl Pts',(-0.21,10.2263890083593,6.51894444366855));
#9446=CARTESIAN_POINT('Ctrl Pts',(-0.204722164681422,10.2545235937782,6.51952376620524));
#9447=CARTESIAN_POINT('Ctrl Pts',(-0.183284867450471,10.3062574468212,6.52161307432363));
#9448=CARTESIAN_POINT('Ctrl Pts',(-0.167126466290584,10.3298583818078,6.52309254589373));
#9449=CARTESIAN_POINT('Ctrl Pts',(-0.129858458976496,10.3671263891219,6.52586721250997));
#9450=CARTESIAN_POINT('Ctrl Pts',(-0.106257490219277,10.3832848505655,6.527343117591));
#9451=CARTESIAN_POINT('Ctrl Pts',(-0.0545235237847863,10.4047221925869,
6.52942425936951));
#9452=CARTESIAN_POINT('Ctrl Pts',(-0.0263888990751172,10.41,6.53));
#9453=CARTESIAN_POINT('Ctrl Pts',(0.0263888990751171,10.41,6.53));
#9454=CARTESIAN_POINT('Ctrl Pts',(0.0545235237847861,10.4047221925869,6.52942425936951));
#9455=CARTESIAN_POINT('Ctrl Pts',(0.106257490219277,10.3832848505655,6.527343117591));
#9456=CARTESIAN_POINT('Ctrl Pts',(0.129858458976496,10.3671263891219,6.52586721250997));
#9457=CARTESIAN_POINT('Ctrl Pts',(0.167126466290584,10.3298583818078,6.52309254589373));
#9458=CARTESIAN_POINT('Ctrl Pts',(0.183284867450471,10.3062574468212,6.52161307432363));
#9459=CARTESIAN_POINT('Ctrl Pts',(0.204722164681422,10.2545235937782,6.51952376620524));
#9460=CARTESIAN_POINT('Ctrl Pts',(0.21,10.2263890083593,6.51894444366855));
#9461=CARTESIAN_POINT('Ctrl Pts',(0.21,10.2,6.51894444366855));
#9462=CARTESIAN_POINT('',(-0.141067359796651,10.355563491861,5.52));
#9463=CARTESIAN_POINT('Origin',(0.,10.2,5.52));
#9464=CARTESIAN_POINT('Ctrl Pts',(0.14106735979665,10.355563491861,5.52));
#9465=CARTESIAN_POINT('Ctrl Pts',(0.123818356698217,10.3712051523632,5.52245784982447));
#9466=CARTESIAN_POINT('Ctrl Pts',(0.102998643109696,10.384624043331,5.52493819304946));
#9467=CARTESIAN_POINT('Ctrl Pts',(0.0546141143983528,10.4046974637244,5.52884449237241));
#9468=CARTESIAN_POINT('Ctrl Pts',(0.0264520736824499,10.41,5.53));
#9469=CARTESIAN_POINT('Ctrl Pts',(-0.0264520736824498,10.41,5.53));
#9470=CARTESIAN_POINT('Ctrl Pts',(-0.0546141143983515,10.4046974637244,
5.52884449237241));
#9471=CARTESIAN_POINT('Ctrl Pts',(-0.102998643109696,10.384624043331,5.52493819304946));
#9472=CARTESIAN_POINT('Ctrl Pts',(-0.123818356698217,10.3712051523632,5.52245784982447));
#9473=CARTESIAN_POINT('Ctrl Pts',(-0.14106735979665,10.355563491861,5.52));
#9474=CARTESIAN_POINT('Origin',(0.,10.2,5.52));
#9475=CARTESIAN_POINT('',(-0.141067359796651,9.,5.52));
#9476=CARTESIAN_POINT('Origin',(-0.3,8.9,3.25));
#9477=CARTESIAN_POINT('',(-0.3,9.,3.25));
#9478=CARTESIAN_POINT('',(-0.3,9.,3.57606079858305));
#9479=CARTESIAN_POINT('',(-0.3,9.,3.89));
#9480=CARTESIAN_POINT('',(-0.3,11.5,3.25));
#9481=CARTESIAN_POINT('',(-0.3,8.9,3.25));
#9482=CARTESIAN_POINT('',(-0.3,11.5,3.57606079858305));
#9483=CARTESIAN_POINT('',(-0.3,11.5,3.89));
#9484=CARTESIAN_POINT('',(-0.3,9.,3.57606079858305));
#9485=CARTESIAN_POINT('Origin',(0.3,8.9,3.25));
#9486=CARTESIAN_POINT('',(0.3,9.,3.25));
#9487=CARTESIAN_POINT('',(0.15,9.,3.25));
#9488=CARTESIAN_POINT('',(0.3,11.5,3.25));
#9489=CARTESIAN_POINT('',(0.3,8.9,3.25));
#9490=CARTESIAN_POINT('',(0.15,11.5,3.25));
#9491=CARTESIAN_POINT('Origin',(0.3,8.9,4.53));
#9492=CARTESIAN_POINT('',(0.3,9.,3.57606079858305));
#9493=CARTESIAN_POINT('',(0.3,9.,4.53));
#9494=CARTESIAN_POINT('',(0.3,11.5,3.57606079858305));
#9495=CARTESIAN_POINT('',(0.3,9.,3.57606079858305));
#9496=CARTESIAN_POINT('',(0.3,11.5,4.53));
#9497=CARTESIAN_POINT('Origin',(0.,11.5,4.53));
#9498=CARTESIAN_POINT('',(-2.,11.5,4.53));
#9499=CARTESIAN_POINT('Origin',(0.,11.5,4.53));
#9500=CARTESIAN_POINT('Origin',(0.,11.5,4.53));
#9501=CARTESIAN_POINT('Origin',(0.,9.,4.53));
#9502=CARTESIAN_POINT('Origin',(0.,9.,4.53));
#9503=CARTESIAN_POINT('Origin',(0.,9.,4.53));
#9504=CARTESIAN_POINT('',(-2.,9.,4.53));
#9505=CARTESIAN_POINT('',(-2.,9.,4.53));
#9506=CARTESIAN_POINT('Origin',(0.,9.,4.53));
#9507=CARTESIAN_POINT('Origin',(0.,9.,4.53));
#9508=CARTESIAN_POINT('',(0.,0.,0.));
#9509=CARTESIAN_POINT('Origin',(0.,-1.25,5.52));
#9510=CARTESIAN_POINT('',(0.172988438920056,-1.36905880899792,5.52));
#9511=CARTESIAN_POINT('',(0.172988438920056,-1.13094119100209,5.52));
#9512=CARTESIAN_POINT('',(0.172988438920056,-1.65,5.52));
#9513=CARTESIAN_POINT('Origin',(0.,-1.25,5.52));
#9514=CARTESIAN_POINT('Origin',(0.,-1.25,5.52));
#9515=CARTESIAN_POINT('',(-0.172988438920056,-1.36905880899792,5.52));
#9516=CARTESIAN_POINT('Ctrl Pts',(-0.172988438920056,-1.36905880899792,
5.52));
#9517=CARTESIAN_POINT('Ctrl Pts',(-0.165594865311314,-1.37980142239529,
5.52129192197638));
#9518=CARTESIAN_POINT('Ctrl Pts',(-0.157297138725606,-1.38968770937274,
5.52265394943905));
#9519=CARTESIAN_POINT('Ctrl Pts',(-0.129892073845076,-1.41709277425327,
5.5267480843909));
#9520=CARTESIAN_POINT('Ctrl Pts',(-0.106330167759284,-1.43324205633295,
5.52969589327638));
#9521=CARTESIAN_POINT('Ctrl Pts',(-0.0546129046324105,-1.45469779396491,
5.53385029472357));
#9522=CARTESIAN_POINT('Ctrl Pts',(-0.0264512308298517,-1.46,5.535));
#9523=CARTESIAN_POINT('Ctrl Pts',(0.0264512308298516,-1.46,5.535));
#9524=CARTESIAN_POINT('Ctrl Pts',(0.0546129046324104,-1.45469779396491,
5.53385029472357));
#9525=CARTESIAN_POINT('Ctrl Pts',(0.106330167759284,-1.43324205633295,5.52969589327638));
#9526=CARTESIAN_POINT('Ctrl Pts',(0.129892073845076,-1.41709277425327,5.5267480843909));
#9527=CARTESIAN_POINT('Ctrl Pts',(0.157297138725606,-1.38968770937274,5.52265394943905));
#9528=CARTESIAN_POINT('Ctrl Pts',(0.165594865311314,-1.37980142239529,5.52129192197638));
#9529=CARTESIAN_POINT('Ctrl Pts',(0.172988438920056,-1.36905880899792,5.52));
#9530=CARTESIAN_POINT('',(-0.21,-1.25,5.52));
#9531=CARTESIAN_POINT('Origin',(0.,-1.25,5.52));
#9532=CARTESIAN_POINT('',(-0.21,-1.25,6.01522725533839));
#9533=CARTESIAN_POINT('',(-0.21,-1.25,5.52));
#9534=CARTESIAN_POINT('',(0.21,-1.25,6.01522725533839));
#9535=CARTESIAN_POINT('Ctrl Pts',(0.21,-1.25,6.01522725533839));
#9536=CARTESIAN_POINT('Ctrl Pts',(0.21,-1.27640552692445,6.01522725533839));
#9537=CARTESIAN_POINT('Ctrl Pts',(0.204715737269596,-1.30454707409071,6.01600415954412));
#9538=CARTESIAN_POINT('Ctrl Pts',(0.183273763036331,-1.35627626890513,6.01880073282317));
#9539=CARTESIAN_POINT('Ctrl Pts',(0.167117923970394,-1.37986692412796,6.02077897157582));
#9540=CARTESIAN_POINT('Ctrl Pts',(0.129867169887369,-1.41711767821098,6.02448481141327));
#9541=CARTESIAN_POINT('Ctrl Pts',(0.106276408305765,-1.43327371000135,6.02645455657129));
#9542=CARTESIAN_POINT('Ctrl Pts',(0.0545468514059002,-1.45471582482622,
6.02923165515645));
#9543=CARTESIAN_POINT('Ctrl Pts',(0.0264051785092814,-1.46,6.03));
#9544=CARTESIAN_POINT('Ctrl Pts',(-0.0264051785092814,-1.46,6.03));
#9545=CARTESIAN_POINT('Ctrl Pts',(-0.0545468514059001,-1.45471582482622,
6.02923165515645));
#9546=CARTESIAN_POINT('Ctrl Pts',(-0.106276408305765,-1.43327371000135,
6.02645455657129));
#9547=CARTESIAN_POINT('Ctrl Pts',(-0.129867169887369,-1.41711767821098,
6.02448481141327));
#9548=CARTESIAN_POINT('Ctrl Pts',(-0.167117923970394,-1.37986692412796,
6.02077897157582));
#9549=CARTESIAN_POINT('Ctrl Pts',(-0.183273763036331,-1.35627626890513,
6.01880073282317));
#9550=CARTESIAN_POINT('Ctrl Pts',(-0.204715737269596,-1.30454707409071,
6.01600415954412));
#9551=CARTESIAN_POINT('Ctrl Pts',(-0.21,-1.27640552692445,6.01522725533839));
#9552=CARTESIAN_POINT('Ctrl Pts',(-0.21,-1.25,6.01522725533839));
#9553=CARTESIAN_POINT('Ctrl Pts',(-0.21,-1.25,6.01522725533839));
#9554=CARTESIAN_POINT('Ctrl Pts',(-0.21,-1.22359447307555,6.01522725533839));
#9555=CARTESIAN_POINT('Ctrl Pts',(-0.204715737269596,-1.19545292590929,
6.01600415954412));
#9556=CARTESIAN_POINT('Ctrl Pts',(-0.183273763036331,-1.14372373109487,
6.01880073282317));
#9557=CARTESIAN_POINT('Ctrl Pts',(-0.167117923970394,-1.12013307587204,
6.02077897157582));
#9558=CARTESIAN_POINT('Ctrl Pts',(-0.129867169887369,-1.08288232178902,
6.02448481141327));
#9559=CARTESIAN_POINT('Ctrl Pts',(-0.106276408305765,-1.06672628999865,
6.02645455657129));
#9560=CARTESIAN_POINT('Ctrl Pts',(-0.0545468514059002,-1.04528417517378,
6.02923165515645));
#9561=CARTESIAN_POINT('Ctrl Pts',(-0.0264051785092814,-1.04,6.03));
#9562=CARTESIAN_POINT('Ctrl Pts',(0.0264051785092814,-1.04,6.03));
#9563=CARTESIAN_POINT('Ctrl Pts',(0.0545468514059001,-1.04528417517378,
6.02923165515645));
#9564=CARTESIAN_POINT('Ctrl Pts',(0.106276408305765,-1.06672628999865,6.02645455657129));
#9565=CARTESIAN_POINT('Ctrl Pts',(0.129867169887369,-1.08288232178902,6.02448481141327));
#9566=CARTESIAN_POINT('Ctrl Pts',(0.167117923970394,-1.12013307587204,6.02077897157582));
#9567=CARTESIAN_POINT('Ctrl Pts',(0.183273763036331,-1.14372373109487,6.01880073282317));
#9568=CARTESIAN_POINT('Ctrl Pts',(0.204715737269596,-1.19545292590929,6.01600415954412));
#9569=CARTESIAN_POINT('Ctrl Pts',(0.21,-1.22359447307555,6.01522725533839));
#9570=CARTESIAN_POINT('Ctrl Pts',(0.21,-1.25,6.01522725533839));
#9571=CARTESIAN_POINT('',(-0.172988438920056,-1.13094119100209,5.52));
#9572=CARTESIAN_POINT('Origin',(0.,-1.25,5.52));
#9573=CARTESIAN_POINT('Ctrl Pts',(0.172988438920056,-1.13094119100209,5.52));
#9574=CARTESIAN_POINT('Ctrl Pts',(0.165594865311315,-1.12019857760471,5.52129192197638));
#9575=CARTESIAN_POINT('Ctrl Pts',(0.157297138725606,-1.11031229062726,5.52265394943905));
#9576=CARTESIAN_POINT('Ctrl Pts',(0.129892073845076,-1.08290722574673,5.5267480843909));
#9577=CARTESIAN_POINT('Ctrl Pts',(0.106330167759284,-1.06675794366705,5.52969589327638));
#9578=CARTESIAN_POINT('Ctrl Pts',(0.0546129046324104,-1.04530220603509,
5.53385029472357));
#9579=CARTESIAN_POINT('Ctrl Pts',(0.0264512308298516,-1.04,5.535));
#9580=CARTESIAN_POINT('Ctrl Pts',(-0.0264512308298516,-1.04,5.535));
#9581=CARTESIAN_POINT('Ctrl Pts',(-0.0546129046324104,-1.04530220603509,
5.53385029472357));
#9582=CARTESIAN_POINT('Ctrl Pts',(-0.106330167759284,-1.06675794366705,
5.52969589327638));
#9583=CARTESIAN_POINT('Ctrl Pts',(-0.129892073845076,-1.08290722574673,
5.5267480843909));
#9584=CARTESIAN_POINT('Ctrl Pts',(-0.157297138725606,-1.11031229062726,
5.52265394943905));
#9585=CARTESIAN_POINT('Ctrl Pts',(-0.165594865311315,-1.12019857760471,
5.52129192197638));
#9586=CARTESIAN_POINT('Ctrl Pts',(-0.172988438920056,-1.13094119100209,
5.52));
#9587=CARTESIAN_POINT('Origin',(0.,-1.25,5.52));
#9588=CARTESIAN_POINT('',(-0.172988438920056,-1.65,5.52));
#9589=CARTESIAN_POINT('Origin',(0.,-1.65,4.53));
#9590=CARTESIAN_POINT('',(-1.005,-0.85,4.53));
#9591=CARTESIAN_POINT('Origin',(0.,-0.85,4.53));
#9592=CARTESIAN_POINT('',(-1.005,-1.65,4.53));
#9593=CARTESIAN_POINT('',(-1.005,-1.65,4.53));
#9594=CARTESIAN_POINT('Origin',(0.,-1.65,4.53));
#9595=CARTESIAN_POINT('Origin',(0.,-1.65,4.53));
#9596=CARTESIAN_POINT('',(-1.5,-0.85,4.53));
#9597=CARTESIAN_POINT('Origin',(0.,-0.85,4.53));
#9598=CARTESIAN_POINT('',(-1.5,-1.65,4.53));
#9599=CARTESIAN_POINT('',(-1.5,-1.65,4.53));
#9600=CARTESIAN_POINT('Origin',(0.,-1.65,4.53));
#9601=CARTESIAN_POINT('Origin',(0.,-0.85,4.53));
#9602=CARTESIAN_POINT('Origin',(0.,-1.65,4.53));
#9603=CARTESIAN_POINT('',(0.,0.,0.));
#9604=CARTESIAN_POINT('Origin',(0.,22.85,5.52));
#9605=CARTESIAN_POINT('',(0.172988438920056,22.7309411910021,5.52));
#9606=CARTESIAN_POINT('',(0.172988438920056,22.9690588089979,5.52));
#9607=CARTESIAN_POINT('',(0.172988438920056,22.45,5.52));
#9608=CARTESIAN_POINT('Origin',(0.,22.85,5.52));
#9609=CARTESIAN_POINT('Origin',(0.,22.85,5.52));
#9610=CARTESIAN_POINT('',(-0.172988438920056,22.7309411910021,5.52));
#9611=CARTESIAN_POINT('Ctrl Pts',(-0.172988438920058,22.7309411910021,5.52));
#9612=CARTESIAN_POINT('Ctrl Pts',(-0.165594865311317,22.7201985776047,5.52129192197638));
#9613=CARTESIAN_POINT('Ctrl Pts',(-0.157297138725606,22.7103122906273,5.52265394943905));
#9614=CARTESIAN_POINT('Ctrl Pts',(-0.129892073845076,22.6829072257467,5.5267480843909));
#9615=CARTESIAN_POINT('Ctrl Pts',(-0.106330167759284,22.6667579436671,5.52969589327638));
#9616=CARTESIAN_POINT('Ctrl Pts',(-0.0546129046324105,22.6453022060351,
5.53385029472357));
#9617=CARTESIAN_POINT('Ctrl Pts',(-0.0264512308298518,22.64,5.535));
#9618=CARTESIAN_POINT('Ctrl Pts',(0.0264512308298517,22.64,5.535));
#9619=CARTESIAN_POINT('Ctrl Pts',(0.0546129046324104,22.6453022060351,5.53385029472357));
#9620=CARTESIAN_POINT('Ctrl Pts',(0.106330167759284,22.6667579436671,5.52969589327638));
#9621=CARTESIAN_POINT('Ctrl Pts',(0.129892073845076,22.6829072257467,5.5267480843909));
#9622=CARTESIAN_POINT('Ctrl Pts',(0.157297138725606,22.7103122906273,5.52265394943905));
#9623=CARTESIAN_POINT('Ctrl Pts',(0.165594865311316,22.7201985776047,5.52129192197638));
#9624=CARTESIAN_POINT('Ctrl Pts',(0.172988438920056,22.7309411910021,5.52));
#9625=CARTESIAN_POINT('',(-0.21,22.85,5.52));
#9626=CARTESIAN_POINT('Origin',(0.,22.85,5.52));
#9627=CARTESIAN_POINT('',(-0.21,22.85,6.01522725533839));
#9628=CARTESIAN_POINT('',(-0.21,22.85,5.52));
#9629=CARTESIAN_POINT('',(0.21,22.85,6.01522725533839));
#9630=CARTESIAN_POINT('Ctrl Pts',(0.21,22.85,6.01522725533839));
#9631=CARTESIAN_POINT('Ctrl Pts',(0.21,22.8235944730755,6.01522725533839));
#9632=CARTESIAN_POINT('Ctrl Pts',(0.204715737269595,22.7954529259093,6.01600415954412));
#9633=CARTESIAN_POINT('Ctrl Pts',(0.18327376303633,22.7437237310949,6.01880073282317));
#9634=CARTESIAN_POINT('Ctrl Pts',(0.167117923970393,22.720133075872,6.02077897157582));
#9635=CARTESIAN_POINT('Ctrl Pts',(0.129867169887369,22.682882321789,6.02448481141327));
#9636=CARTESIAN_POINT('Ctrl Pts',(0.106276408305767,22.6667262899986,6.02645455657129));
#9637=CARTESIAN_POINT('Ctrl Pts',(0.054546851405902,22.6452841751738,6.02923165515645));
#9638=CARTESIAN_POINT('Ctrl Pts',(0.0264051785092816,22.64,6.03));
#9639=CARTESIAN_POINT('Ctrl Pts',(-0.0264051785092815,22.64,6.03));
#9640=CARTESIAN_POINT('Ctrl Pts',(-0.0545468514059018,22.6452841751738,
6.02923165515645));
#9641=CARTESIAN_POINT('Ctrl Pts',(-0.106276408305767,22.6667262899986,6.02645455657129));
#9642=CARTESIAN_POINT('Ctrl Pts',(-0.129867169887368,22.682882321789,6.02448481141327));
#9643=CARTESIAN_POINT('Ctrl Pts',(-0.167117923970393,22.720133075872,6.02077897157582));
#9644=CARTESIAN_POINT('Ctrl Pts',(-0.183273763036334,22.7437237310949,6.01880073282317));
#9645=CARTESIAN_POINT('Ctrl Pts',(-0.204715737269596,22.7954529259093,6.01600415954412));
#9646=CARTESIAN_POINT('Ctrl Pts',(-0.21,22.8235944730755,6.01522725533839));
#9647=CARTESIAN_POINT('Ctrl Pts',(-0.21,22.85,6.01522725533839));
#9648=CARTESIAN_POINT('Ctrl Pts',(-0.21,22.85,6.01522725533839));
#9649=CARTESIAN_POINT('Ctrl Pts',(-0.21,22.8764055269245,6.01522725533839));
#9650=CARTESIAN_POINT('Ctrl Pts',(-0.204715737269595,22.9045470740907,6.01600415954412));
#9651=CARTESIAN_POINT('Ctrl Pts',(-0.18327376303633,22.9562762689051,6.01880073282317));
#9652=CARTESIAN_POINT('Ctrl Pts',(-0.167117923970393,22.979866924128,6.02077897157582));
#9653=CARTESIAN_POINT('Ctrl Pts',(-0.129867169887369,23.017117678211,6.02448481141327));
#9654=CARTESIAN_POINT('Ctrl Pts',(-0.106276408305767,23.0332737100014,6.02645455657129));
#9655=CARTESIAN_POINT('Ctrl Pts',(-0.054546851405902,23.0547158248262,6.02923165515645));
#9656=CARTESIAN_POINT('Ctrl Pts',(-0.0264051785092816,23.06,6.03));
#9657=CARTESIAN_POINT('Ctrl Pts',(0.0264051785092815,23.06,6.03));
#9658=CARTESIAN_POINT('Ctrl Pts',(0.0545468514059019,23.0547158248262,6.02923165515645));
#9659=CARTESIAN_POINT('Ctrl Pts',(0.106276408305767,23.0332737100014,6.02645455657129));
#9660=CARTESIAN_POINT('Ctrl Pts',(0.129867169887368,23.017117678211,6.02448481141327));
#9661=CARTESIAN_POINT('Ctrl Pts',(0.167117923970393,22.979866924128,6.02077897157582));
#9662=CARTESIAN_POINT('Ctrl Pts',(0.18327376303633,22.9562762689051,6.01880073282317));
#9663=CARTESIAN_POINT('Ctrl Pts',(0.204715737269595,22.9045470740907,6.01600415954412));
#9664=CARTESIAN_POINT('Ctrl Pts',(0.21,22.8764055269245,6.01522725533839));
#9665=CARTESIAN_POINT('Ctrl Pts',(0.21,22.85,6.01522725533839));
#9666=CARTESIAN_POINT('',(-0.172988438920056,22.9690588089979,5.52));
#9667=CARTESIAN_POINT('Origin',(0.,22.85,5.52));
#9668=CARTESIAN_POINT('Ctrl Pts',(0.172988438920055,22.9690588089979,5.52));
#9669=CARTESIAN_POINT('Ctrl Pts',(0.165594865311314,22.9798014223953,5.52129192197638));
#9670=CARTESIAN_POINT('Ctrl Pts',(0.157297138725605,22.9896877093727,5.52265394943905));
#9671=CARTESIAN_POINT('Ctrl Pts',(0.129892073845076,23.0170927742533,5.5267480843909));
#9672=CARTESIAN_POINT('Ctrl Pts',(0.106330167759284,23.033242056333,5.52969589327638));
#9673=CARTESIAN_POINT('Ctrl Pts',(0.0546129046324105,23.0546977939649,5.53385029472357));
#9674=CARTESIAN_POINT('Ctrl Pts',(0.0264512308298518,23.06,5.535));
#9675=CARTESIAN_POINT('Ctrl Pts',(-0.0264512308298517,23.06,5.535));
#9676=CARTESIAN_POINT('Ctrl Pts',(-0.0546129046324079,23.0546977939649,
5.53385029472357));
#9677=CARTESIAN_POINT('Ctrl Pts',(-0.106330167759282,23.033242056333,5.52969589327638));
#9678=CARTESIAN_POINT('Ctrl Pts',(-0.129892073845076,23.0170927742533,5.5267480843909));
#9679=CARTESIAN_POINT('Ctrl Pts',(-0.157297138725605,22.9896877093727,5.52265394943905));
#9680=CARTESIAN_POINT('Ctrl Pts',(-0.165594865311314,22.9798014223953,5.52129192197638));
#9681=CARTESIAN_POINT('Ctrl Pts',(-0.172988438920055,22.9690588089979,5.52));
#9682=CARTESIAN_POINT('Origin',(0.,22.85,5.52));
#9683=CARTESIAN_POINT('',(-0.172988438920056,22.45,5.52));
#9684=CARTESIAN_POINT('Origin',(0.,22.45,4.53));
#9685=CARTESIAN_POINT('',(-1.005,23.25,4.53));
#9686=CARTESIAN_POINT('Origin',(0.,23.25,4.53));
#9687=CARTESIAN_POINT('',(-1.005,22.45,4.53));
#9688=CARTESIAN_POINT('',(-1.005,22.45,4.53));
#9689=CARTESIAN_POINT('Origin',(0.,22.45,4.53));
#9690=CARTESIAN_POINT('Origin',(0.,22.45,4.53));
#9691=CARTESIAN_POINT('',(-1.5,23.25,4.53));
#9692=CARTESIAN_POINT('Origin',(0.,23.25,4.53));
#9693=CARTESIAN_POINT('',(-1.5,22.45,4.53));
#9694=CARTESIAN_POINT('',(-1.5,22.45,4.53));
#9695=CARTESIAN_POINT('Origin',(0.,22.45,4.53));
#9696=CARTESIAN_POINT('Origin',(0.,23.25,4.53));
#9697=CARTESIAN_POINT('Origin',(0.,22.45,4.53));
#9698=CARTESIAN_POINT('',(0.,0.,0.));
#9699=CARTESIAN_POINT('Origin',(-0.2,-1.,-0.78));
#9700=CARTESIAN_POINT('',(-0.2,-0.9,-0.78));
#9701=CARTESIAN_POINT('',(-0.2,-0.9,-0.565685424949238));
#9702=CARTESIAN_POINT('',(-0.2,-0.9,-0.39));
#9703=CARTESIAN_POINT('',(-0.2,0.85,-0.78));
#9704=CARTESIAN_POINT('',(-0.2,-1.,-0.78));
#9705=CARTESIAN_POINT('',(-0.2,0.85,-0.565685424949238));
#9706=CARTESIAN_POINT('',(-0.2,0.85,-0.39));
#9707=CARTESIAN_POINT('',(-0.2,0.,-0.565685424949238));
#9708=CARTESIAN_POINT('Origin',(0.2,-1.,-0.78));
#9709=CARTESIAN_POINT('',(0.2,-0.9,-0.78));
#9710=CARTESIAN_POINT('',(0.1,-0.9,-0.78));
#9711=CARTESIAN_POINT('',(0.2,0.85,-0.78));
#9712=CARTESIAN_POINT('',(0.2,-1.,-0.78));
#9713=CARTESIAN_POINT('',(0.1,0.85,-0.78));
#9714=CARTESIAN_POINT('',(-0.125,-0.5,-0.78));
#9715=CARTESIAN_POINT('Origin',(0.,-0.5,-0.78));
#9716=CARTESIAN_POINT('Origin',(0.2,-1.,0.));
#9717=CARTESIAN_POINT('',(0.2,-0.9,-0.565685424949238));
#9718=CARTESIAN_POINT('',(0.2,-0.9,0.));
#9719=CARTESIAN_POINT('',(0.2,0.85,-0.565685424949238));
#9720=CARTESIAN_POINT('',(0.2,0.,-0.565685424949238));
#9721=CARTESIAN_POINT('',(0.2,0.85,0.));
#9722=CARTESIAN_POINT('Origin',(0.,0.85,0.));
#9723=CARTESIAN_POINT('',(-1.4,0.85,1.71450551880629E-16));
#9724=CARTESIAN_POINT('Origin',(0.,0.85,0.));
#9725=CARTESIAN_POINT('Origin',(0.,0.85,0.));
#9726=CARTESIAN_POINT('Origin',(0.,0.,0.));
#9727=CARTESIAN_POINT('Origin',(0.,-0.9,0.));
#9728=CARTESIAN_POINT('',(0.125,-0.5,0.586834729715275));
#9729=CARTESIAN_POINT('',(-0.125,-0.5,0.586834729715275));
#9730=CARTESIAN_POINT('Ctrl Pts',(0.125,-0.5,0.586834729715275));
#9731=CARTESIAN_POINT('Ctrl Pts',(0.125,-0.484254474936005,0.586834729715275));
#9732=CARTESIAN_POINT('Ctrl Pts',(0.121843784097853,-0.467492086231842,
0.587534197873268));
#9733=CARTESIAN_POINT('Ctrl Pts',(0.109073016834181,-0.436709004341607,
0.590038488226116));
#9734=CARTESIAN_POINT('Ctrl Pts',(0.0994608796208941,-0.422684184324257,
0.591804743154611));
#9735=CARTESIAN_POINT('Ctrl Pts',(0.077316548567853,-0.400539853271216,
0.59510289473619));
#9736=CARTESIAN_POINT('Ctrl Pts',(0.0632914182239686,-0.390927142361291,
0.596852269967858));
#9737=CARTESIAN_POINT('Ctrl Pts',(0.0325072544867634,-0.378155958502111,
0.599317707212167));
#9738=CARTESIAN_POINT('Ctrl Pts',(0.0157444828659572,-0.375,0.6));
#9739=CARTESIAN_POINT('Ctrl Pts',(-0.0157444828659573,-0.375,0.6));
#9740=CARTESIAN_POINT('Ctrl Pts',(-0.0325072544867634,-0.378155958502111,
0.599317707212167));
#9741=CARTESIAN_POINT('Ctrl Pts',(-0.0632914182239687,-0.390927142361291,
0.596852269967858));
#9742=CARTESIAN_POINT('Ctrl Pts',(-0.077316548567853,-0.400539853271216,
0.59510289473619));
#9743=CARTESIAN_POINT('Ctrl Pts',(-0.0994608796208942,-0.422684184324257,
0.591804743154611));
#9744=CARTESIAN_POINT('Ctrl Pts',(-0.109073016834181,-0.436709004341607,
0.590038488226116));
#9745=CARTESIAN_POINT('Ctrl Pts',(-0.121843784097853,-0.467492086231842,
0.587534197873268));
#9746=CARTESIAN_POINT('Ctrl Pts',(-0.125,-0.484254474936005,0.586834729715275));
#9747=CARTESIAN_POINT('Ctrl Pts',(-0.125,-0.5,0.586834729715275));
#9748=CARTESIAN_POINT('Ctrl Pts',(-0.125,-0.5,0.586834729715275));
#9749=CARTESIAN_POINT('Ctrl Pts',(-0.125,-0.515745525063995,0.586834729715275));
#9750=CARTESIAN_POINT('Ctrl Pts',(-0.121843784097853,-0.532507913768158,
0.587534197873268));
#9751=CARTESIAN_POINT('Ctrl Pts',(-0.109073016834181,-0.563290995658393,
0.590038488226116));
#9752=CARTESIAN_POINT('Ctrl Pts',(-0.0994608796208941,-0.577315815675743,
0.591804743154611));
#9753=CARTESIAN_POINT('Ctrl Pts',(-0.077316548567853,-0.599460146728784,
0.59510289473619));
#9754=CARTESIAN_POINT('Ctrl Pts',(-0.0632914182239687,-0.609072857638709,
0.596852269967858));
#9755=CARTESIAN_POINT('Ctrl Pts',(-0.0325072544867635,-0.621844041497889,
0.599317707212167));
#9756=CARTESIAN_POINT('Ctrl Pts',(-0.0157444828659572,-0.625,0.6));
#9757=CARTESIAN_POINT('Ctrl Pts',(0.0157444828659572,-0.625,0.6));
#9758=CARTESIAN_POINT('Ctrl Pts',(0.0325072544867633,-0.621844041497889,
0.599317707212167));
#9759=CARTESIAN_POINT('Ctrl Pts',(0.0632914182239686,-0.609072857638709,
0.596852269967858));
#9760=CARTESIAN_POINT('Ctrl Pts',(0.077316548567853,-0.599460146728784,
0.59510289473619));
#9761=CARTESIAN_POINT('Ctrl Pts',(0.0994608796208942,-0.577315815675743,
0.591804743154611));
#9762=CARTESIAN_POINT('Ctrl Pts',(0.109073016834181,-0.563290995658393,
0.590038488226116));
#9763=CARTESIAN_POINT('Ctrl Pts',(0.121843784097853,-0.532507913768158,
0.587534197873268));
#9764=CARTESIAN_POINT('Ctrl Pts',(0.125,-0.515745525063995,0.586834729715275));
#9765=CARTESIAN_POINT('Ctrl Pts',(0.125,-0.5,0.586834729715275));
#9766=CARTESIAN_POINT('',(-0.586834729715275,-0.5,-0.125));
#9767=CARTESIAN_POINT('',(-0.586834729715275,-0.5,0.125));
#9768=CARTESIAN_POINT('Ctrl Pts',(-0.586834729715275,-0.5,-0.125));
#9769=CARTESIAN_POINT('Ctrl Pts',(-0.586834729715275,-0.515745525063995,
-0.125));
#9770=CARTESIAN_POINT('Ctrl Pts',(-0.587534197873268,-0.532507913768158,
-0.121843784097853));
#9771=CARTESIAN_POINT('Ctrl Pts',(-0.590038488226116,-0.563290995658393,
-0.109073016834181));
#9772=CARTESIAN_POINT('Ctrl Pts',(-0.591804743154611,-0.577315815675743,
-0.0994608796208942));
#9773=CARTESIAN_POINT('Ctrl Pts',(-0.59510289473619,-0.599460146728784,
-0.0773165485678531));
#9774=CARTESIAN_POINT('Ctrl Pts',(-0.596852269967858,-0.609072857638709,
-0.0632914182239687));
#9775=CARTESIAN_POINT('Ctrl Pts',(-0.599317707212167,-0.621844041497889,
-0.0325072544867635));
#9776=CARTESIAN_POINT('Ctrl Pts',(-0.6,-0.625,-0.0157444828659573));
#9777=CARTESIAN_POINT('Ctrl Pts',(-0.6,-0.625,0.0157444828659572));
#9778=CARTESIAN_POINT('Ctrl Pts',(-0.599317707212167,-0.621844041497889,
0.0325072544867633));
#9779=CARTESIAN_POINT('Ctrl Pts',(-0.596852269967858,-0.609072857638709,
0.0632914182239686));
#9780=CARTESIAN_POINT('Ctrl Pts',(-0.59510289473619,-0.599460146728784,
0.077316548567853));
#9781=CARTESIAN_POINT('Ctrl Pts',(-0.591804743154611,-0.577315815675743,
0.0994608796208941));
#9782=CARTESIAN_POINT('Ctrl Pts',(-0.590038488226116,-0.563290995658393,
0.109073016834181));
#9783=CARTESIAN_POINT('Ctrl Pts',(-0.587534197873268,-0.532507913768158,
0.121843784097853));
#9784=CARTESIAN_POINT('Ctrl Pts',(-0.586834729715275,-0.515745525063995,
0.125));
#9785=CARTESIAN_POINT('Ctrl Pts',(-0.586834729715275,-0.5,0.125));
#9786=CARTESIAN_POINT('Ctrl Pts',(-0.586834729715275,-0.5,0.125));
#9787=CARTESIAN_POINT('Ctrl Pts',(-0.586834729715275,-0.484254474936005,
0.125));
#9788=CARTESIAN_POINT('Ctrl Pts',(-0.587534197873268,-0.467492086231842,
0.121843784097853));
#9789=CARTESIAN_POINT('Ctrl Pts',(-0.590038488226116,-0.436709004341607,
0.109073016834181));
#9790=CARTESIAN_POINT('Ctrl Pts',(-0.591804743154611,-0.422684184324257,
0.0994608796208941));
#9791=CARTESIAN_POINT('Ctrl Pts',(-0.59510289473619,-0.400539853271216,
0.077316548567853));
#9792=CARTESIAN_POINT('Ctrl Pts',(-0.596852269967858,-0.390927142361291,
0.0632914182239686));
#9793=CARTESIAN_POINT('Ctrl Pts',(-0.599317707212167,-0.378155958502111,
0.0325072544867634));
#9794=CARTESIAN_POINT('Ctrl Pts',(-0.6,-0.375,0.0157444828659572));
#9795=CARTESIAN_POINT('Ctrl Pts',(-0.6,-0.375,-0.0157444828659572));
#9796=CARTESIAN_POINT('Ctrl Pts',(-0.599317707212167,-0.378155958502111,
-0.0325072544867634));
#9797=CARTESIAN_POINT('Ctrl Pts',(-0.596852269967858,-0.390927142361291,
-0.0632914182239686));
#9798=CARTESIAN_POINT('Ctrl Pts',(-0.59510289473619,-0.400539853271216,
-0.077316548567853));
#9799=CARTESIAN_POINT('Ctrl Pts',(-0.591804743154611,-0.422684184324257,
-0.0994608796208942));
#9800=CARTESIAN_POINT('Ctrl Pts',(-0.590038488226116,-0.436709004341607,
-0.109073016834181));
#9801=CARTESIAN_POINT('Ctrl Pts',(-0.587534197873268,-0.467492086231842,
-0.121843784097853));
#9802=CARTESIAN_POINT('Ctrl Pts',(-0.586834729715275,-0.484254474936005,
-0.125));
#9803=CARTESIAN_POINT('Ctrl Pts',(-0.586834729715275,-0.5,-0.125));
#9804=CARTESIAN_POINT('',(0.586834729715275,-0.5,-0.125));
#9805=CARTESIAN_POINT('',(0.586834729715275,-0.5,0.125));
#9806=CARTESIAN_POINT('Ctrl Pts',(0.586834729715275,-0.5,-0.125));
#9807=CARTESIAN_POINT('Ctrl Pts',(0.586834729715275,-0.484254474936005,
-0.125));
#9808=CARTESIAN_POINT('Ctrl Pts',(0.587534197873268,-0.467492086231842,
-0.121843784097853));
#9809=CARTESIAN_POINT('Ctrl Pts',(0.590038488226116,-0.436709004341607,
-0.109073016834181));
#9810=CARTESIAN_POINT('Ctrl Pts',(0.591804743154611,-0.422684184324257,
-0.0994608796208941));
#9811=CARTESIAN_POINT('Ctrl Pts',(0.59510289473619,-0.400539853271216,-0.0773165485678529));
#9812=CARTESIAN_POINT('Ctrl Pts',(0.596852269967858,-0.390927142361291,
-0.0632914182239686));
#9813=CARTESIAN_POINT('Ctrl Pts',(0.599317707212167,-0.378155958502111,
-0.0325072544867633));
#9814=CARTESIAN_POINT('Ctrl Pts',(0.6,-0.375,-0.0157444828659572));
#9815=CARTESIAN_POINT('Ctrl Pts',(0.6,-0.375,0.0157444828659573));
#9816=CARTESIAN_POINT('Ctrl Pts',(0.599317707212167,-0.378155958502111,
0.0325072544867635));
#9817=CARTESIAN_POINT('Ctrl Pts',(0.596852269967858,-0.390927142361291,
0.0632914182239687));
#9818=CARTESIAN_POINT('Ctrl Pts',(0.59510289473619,-0.400539853271216,0.0773165485678531));
#9819=CARTESIAN_POINT('Ctrl Pts',(0.591804743154611,-0.422684184324257,
0.0994608796208942));
#9820=CARTESIAN_POINT('Ctrl Pts',(0.590038488226116,-0.436709004341607,
0.109073016834181));
#9821=CARTESIAN_POINT('Ctrl Pts',(0.587534197873268,-0.467492086231842,
0.121843784097853));
#9822=CARTESIAN_POINT('Ctrl Pts',(0.586834729715275,-0.484254474936005,
0.125));
#9823=CARTESIAN_POINT('Ctrl Pts',(0.586834729715275,-0.5,0.125));
#9824=CARTESIAN_POINT('Ctrl Pts',(0.586834729715275,-0.5,0.125));
#9825=CARTESIAN_POINT('Ctrl Pts',(0.586834729715275,-0.515745525063995,
0.125));
#9826=CARTESIAN_POINT('Ctrl Pts',(0.587534197873268,-0.532507913768158,
0.121843784097853));
#9827=CARTESIAN_POINT('Ctrl Pts',(0.590038488226116,-0.563290995658393,
0.109073016834181));
#9828=CARTESIAN_POINT('Ctrl Pts',(0.591804743154611,-0.577315815675743,
0.0994608796208942));
#9829=CARTESIAN_POINT('Ctrl Pts',(0.59510289473619,-0.599460146728784,0.077316548567853));
#9830=CARTESIAN_POINT('Ctrl Pts',(0.596852269967858,-0.609072857638709,
0.0632914182239688));
#9831=CARTESIAN_POINT('Ctrl Pts',(0.599317707212167,-0.621844041497889,
0.0325072544867635));
#9832=CARTESIAN_POINT('Ctrl Pts',(0.6,-0.625,0.0157444828659573));
#9833=CARTESIAN_POINT('Ctrl Pts',(0.6,-0.625,-0.0157444828659572));
#9834=CARTESIAN_POINT('Ctrl Pts',(0.599317707212167,-0.621844041497889,
-0.0325072544867633));
#9835=CARTESIAN_POINT('Ctrl Pts',(0.596852269967858,-0.609072857638709,
-0.0632914182239685));
#9836=CARTESIAN_POINT('Ctrl Pts',(0.59510289473619,-0.599460146728784,-0.077316548567853));
#9837=CARTESIAN_POINT('Ctrl Pts',(0.591804743154611,-0.577315815675743,
-0.0994608796208941));
#9838=CARTESIAN_POINT('Ctrl Pts',(0.590038488226116,-0.563290995658393,
-0.10907301683418));
#9839=CARTESIAN_POINT('Ctrl Pts',(0.587534197873268,-0.532507913768158,
-0.121843784097853));
#9840=CARTESIAN_POINT('Ctrl Pts',(0.586834729715275,-0.515745525063995,
-0.125));
#9841=CARTESIAN_POINT('Ctrl Pts',(0.586834729715275,-0.5,-0.125));
#9842=CARTESIAN_POINT('Origin',(0.,-0.5,0.));
#9843=CARTESIAN_POINT('',(-1.,-0.375,-6.12323399573677E-17));
#9844=CARTESIAN_POINT('',(-0.992156741649222,-0.5,0.125));
#9845=CARTESIAN_POINT('Ctrl Pts',(-1.,-0.375,-1.00613961606655E-16));
#9846=CARTESIAN_POINT('Ctrl Pts',(-1.,-0.375,0.0157128711428661));
#9847=CARTESIAN_POINT('Ctrl Pts',(-0.999591823858855,-0.378143583103513,
0.0324619190698278));
#9848=CARTESIAN_POINT('Ctrl Pts',(-0.998116453123232,-0.390905426591754,
0.0632545375991437));
#9849=CARTESIAN_POINT('Ctrl Pts',(-0.997070068816062,-0.400522781657727,
0.0772994769543643));
#9850=CARTESIAN_POINT('Ctrl Pts',(-0.995102104277285,-0.422700615683787,
0.0994773109804239));
#9851=CARTESIAN_POINT('Ctrl Pts',(-0.994052129228928,-0.436745514765346,
0.109094593469654));
#9852=CARTESIAN_POINT('Ctrl Pts',(-0.99256853061881,-0.467537996927464,
0.121856383722779));
#9853=CARTESIAN_POINT('Ctrl Pts',(-0.992156741649222,-0.484286997589363,
0.125));
#9854=CARTESIAN_POINT('Ctrl Pts',(-0.992156741649222,-0.5,0.125));
#9855=CARTESIAN_POINT('',(-1.,-0.625,-6.12323399573677E-17));
#9856=CARTESIAN_POINT('Ctrl Pts',(-1.,-0.625,-4.5102810375397E-17));
#9857=CARTESIAN_POINT('Ctrl Pts',(-1.,-0.625,-0.0157128711428662));
#9858=CARTESIAN_POINT('Ctrl Pts',(-0.999591823858855,-0.621856416896487,
-0.032461919069828));
#9859=CARTESIAN_POINT('Ctrl Pts',(-0.998116453123232,-0.609094573408246,
-0.0632545375991439));
#9860=CARTESIAN_POINT('Ctrl Pts',(-0.997070068816062,-0.599477218342273,
-0.0772994769543645));
#9861=CARTESIAN_POINT('Ctrl Pts',(-0.995102104277285,-0.577299384316213,
-0.0994773109804241));
#9862=CARTESIAN_POINT('Ctrl Pts',(-0.994052129228928,-0.563254485234654,
-0.109094593469655));
#9863=CARTESIAN_POINT('Ctrl Pts',(-0.99256853061881,-0.532462003072536,
-0.121856383722779));
#9864=CARTESIAN_POINT('Ctrl Pts',(-0.992156741649221,-0.515713002410637,
-0.125));
#9865=CARTESIAN_POINT('Ctrl Pts',(-0.992156741649221,-0.484286997589363,
-0.125));
#9866=CARTESIAN_POINT('Ctrl Pts',(-0.99256853061881,-0.467537996927464,
-0.121856383722779));
#9867=CARTESIAN_POINT('Ctrl Pts',(-0.994052129228928,-0.436745514765346,
-0.109094593469655));
#9868=CARTESIAN_POINT('Ctrl Pts',(-0.995102104277285,-0.422700615683787,
-0.0994773109804241));
#9869=CARTESIAN_POINT('Ctrl Pts',(-0.997070068816062,-0.400522781657728,
-0.0772994769543645));
#9870=CARTESIAN_POINT('Ctrl Pts',(-0.998116453123232,-0.390905426591754,
-0.063254537599144));
#9871=CARTESIAN_POINT('Ctrl Pts',(-0.999591823858855,-0.378143583103513,
-0.0324619190698281));
#9872=CARTESIAN_POINT('Ctrl Pts',(-1.,-0.375,-0.0157128711428663));
#9873=CARTESIAN_POINT('Ctrl Pts',(-1.,-0.375,-9.36750677027476E-17));
#9874=CARTESIAN_POINT('Ctrl Pts',(-0.992156741649222,-0.5,0.125));
#9875=CARTESIAN_POINT('Ctrl Pts',(-0.992156741649222,-0.515713002410637,
0.125));
#9876=CARTESIAN_POINT('Ctrl Pts',(-0.99256853061881,-0.532462003072536,
0.121856383722779));
#9877=CARTESIAN_POINT('Ctrl Pts',(-0.994052129228928,-0.563254485234654,
0.109094593469654));
#9878=CARTESIAN_POINT('Ctrl Pts',(-0.995102104277285,-0.577299384316213,
0.0994773109804241));
#9879=CARTESIAN_POINT('Ctrl Pts',(-0.997070068816062,-0.599477218342273,
0.0772994769543644));
#9880=CARTESIAN_POINT('Ctrl Pts',(-0.998116453123232,-0.609094573408246,
0.0632545375991438));
#9881=CARTESIAN_POINT('Ctrl Pts',(-0.999591823858855,-0.621856416896487,
0.0324619190698279));
#9882=CARTESIAN_POINT('Ctrl Pts',(-1.,-0.625,0.0157128711428661));
#9883=CARTESIAN_POINT('Ctrl Pts',(-1.,-0.625,-4.85722573273506E-17));
#9884=CARTESIAN_POINT('',(-7.65404249467096E-18,-0.5,0.125));
#9885=CARTESIAN_POINT('Origin',(0.,-0.5,0.));
#9886=CARTESIAN_POINT('',(0.992156741649222,-0.5,0.125));
#9887=CARTESIAN_POINT('',(-7.65404249467096E-18,-0.5,0.125));
#9888=CARTESIAN_POINT('',(1.,-0.625,6.12323399573677E-17));
#9889=CARTESIAN_POINT('Ctrl Pts',(1.,-0.625,7.28583859910259E-17));
#9890=CARTESIAN_POINT('Ctrl Pts',(1.,-0.625,0.0157128711428663));
#9891=CARTESIAN_POINT('Ctrl Pts',(0.999591823858855,-0.621856416896487,
0.032461919069828));
#9892=CARTESIAN_POINT('Ctrl Pts',(0.998116453123232,-0.609094573408246,
0.0632545375991439));
#9893=CARTESIAN_POINT('Ctrl Pts',(0.997070068816062,-0.599477218342273,
0.0772994769543645));
#9894=CARTESIAN_POINT('Ctrl Pts',(0.995102104277285,-0.577299384316213,
0.0994773109804242));
#9895=CARTESIAN_POINT('Ctrl Pts',(0.994052129228928,-0.563254485234654,
0.109094593469655));
#9896=CARTESIAN_POINT('Ctrl Pts',(0.99256853061881,-0.532462003072536,0.121856383722779));
#9897=CARTESIAN_POINT('Ctrl Pts',(0.992156741649222,-0.515713002410637,
0.125));
#9898=CARTESIAN_POINT('Ctrl Pts',(0.992156741649222,-0.5,0.125));
#9899=CARTESIAN_POINT('',(1.,-0.375,6.12323399573677E-17));
#9900=CARTESIAN_POINT('Ctrl Pts',(1.,-0.375,2.08166817117217E-17));
#9901=CARTESIAN_POINT('Ctrl Pts',(1.,-0.375,-0.0157128711428662));
#9902=CARTESIAN_POINT('Ctrl Pts',(0.999591823858855,-0.378143583103513,
-0.032461919069828));
#9903=CARTESIAN_POINT('Ctrl Pts',(0.998116453123232,-0.390905426591754,
-0.0632545375991438));
#9904=CARTESIAN_POINT('Ctrl Pts',(0.997070068816062,-0.400522781657728,
-0.0772994769543644));
#9905=CARTESIAN_POINT('Ctrl Pts',(0.995102104277285,-0.422700615683787,
-0.099477310980424));
#9906=CARTESIAN_POINT('Ctrl Pts',(0.994052129228928,-0.436745514765346,
-0.109094593469654));
#9907=CARTESIAN_POINT('Ctrl Pts',(0.99256853061881,-0.467537996927464,-0.121856383722779));
#9908=CARTESIAN_POINT('Ctrl Pts',(0.992156741649222,-0.484286997589363,
-0.125));
#9909=CARTESIAN_POINT('Ctrl Pts',(0.992156741649222,-0.515713002410637,
-0.125));
#9910=CARTESIAN_POINT('Ctrl Pts',(0.99256853061881,-0.532462003072536,-0.121856383722779));
#9911=CARTESIAN_POINT('Ctrl Pts',(0.994052129228928,-0.563254485234654,
-0.109094593469654));
#9912=CARTESIAN_POINT('Ctrl Pts',(0.995102104277285,-0.577299384316213,
-0.099477310980424));
#9913=CARTESIAN_POINT('Ctrl Pts',(0.997070068816062,-0.599477218342273,
-0.0772994769543643));
#9914=CARTESIAN_POINT('Ctrl Pts',(0.998116453123232,-0.609094573408246,
-0.0632545375991438));
#9915=CARTESIAN_POINT('Ctrl Pts',(0.999591823858855,-0.621856416896487,
-0.0324619190698279));
#9916=CARTESIAN_POINT('Ctrl Pts',(1.,-0.625,-0.0157128711428661));
#9917=CARTESIAN_POINT('Ctrl Pts',(1.,-0.625,8.32667268468867E-17));
#9918=CARTESIAN_POINT('Ctrl Pts',(0.992156741649222,-0.5,0.125));
#9919=CARTESIAN_POINT('Ctrl Pts',(0.992156741649222,-0.484286997589363,
0.125));
#9920=CARTESIAN_POINT('Ctrl Pts',(0.99256853061881,-0.467537996927464,0.121856383722779));
#9921=CARTESIAN_POINT('Ctrl Pts',(0.994052129228928,-0.436745514765346,
0.109094593469654));
#9922=CARTESIAN_POINT('Ctrl Pts',(0.995102104277285,-0.422700615683787,
0.0994773109804241));
#9923=CARTESIAN_POINT('Ctrl Pts',(0.997070068816062,-0.400522781657727,
0.0772994769543644));
#9924=CARTESIAN_POINT('Ctrl Pts',(0.998116453123232,-0.390905426591754,
0.0632545375991438));
#9925=CARTESIAN_POINT('Ctrl Pts',(0.999591823858855,-0.378143583103513,
0.0324619190698279));
#9926=CARTESIAN_POINT('Ctrl Pts',(1.,-0.375,0.0157128711428662));
#9927=CARTESIAN_POINT('Ctrl Pts',(1.,-0.375,2.77555756156289E-17));
#9928=CARTESIAN_POINT('Origin',(0.,-0.1,0.));
#9929=CARTESIAN_POINT('',(-1.,-0.9,1.22464679914735E-16));
#9930=CARTESIAN_POINT('Origin',(0.,-0.9,0.));
#9931=CARTESIAN_POINT('',(-1.,-0.1,-1.22464679914735E-16));
#9932=CARTESIAN_POINT('',(-1.,-0.1,1.22464679914735E-16));
#9933=CARTESIAN_POINT('',(-1.,-0.1,-1.22464679914735E-16));
#9934=CARTESIAN_POINT('Origin',(0.,-0.1,0.));
#9935=CARTESIAN_POINT('',(0.,-0.625,-1.));
#9936=CARTESIAN_POINT('',(0.,-0.375,-1.));
#9937=CARTESIAN_POINT('Ctrl Pts',(-2.08166817117217E-17,-0.625,-1.));
#9938=CARTESIAN_POINT('Ctrl Pts',(0.0157128711428662,-0.625,-1.));
#9939=CARTESIAN_POINT('Ctrl Pts',(0.0324619190698279,-0.621856416896487,
-0.999591823858855));
#9940=CARTESIAN_POINT('Ctrl Pts',(0.0632545375991438,-0.609094573408246,
-0.998116453123232));
#9941=CARTESIAN_POINT('Ctrl Pts',(0.0772994769543644,-0.599477218342273,
-0.997070068816062));
#9942=CARTESIAN_POINT('Ctrl Pts',(0.0994773109804241,-0.577299384316213,
-0.995102104277285));
#9943=CARTESIAN_POINT('Ctrl Pts',(0.109094593469654,-0.563254485234654,
-0.994052129228928));
#9944=CARTESIAN_POINT('Ctrl Pts',(0.121856383722779,-0.532462003072536,
-0.99256853061881));
#9945=CARTESIAN_POINT('Ctrl Pts',(0.125,-0.515713002410637,-0.992156741649221));
#9946=CARTESIAN_POINT('Ctrl Pts',(0.125,-0.484286997589363,-0.992156741649221));
#9947=CARTESIAN_POINT('Ctrl Pts',(0.121856383722779,-0.467537996927464,
-0.99256853061881));
#9948=CARTESIAN_POINT('Ctrl Pts',(0.109094593469654,-0.436745514765346,
-0.994052129228928));
#9949=CARTESIAN_POINT('Ctrl Pts',(0.0994773109804241,-0.422700615683787,
-0.995102104277285));
#9950=CARTESIAN_POINT('Ctrl Pts',(0.0772994769543645,-0.400522781657728,
-0.997070068816062));
#9951=CARTESIAN_POINT('Ctrl Pts',(0.0632545375991439,-0.390905426591754,
-0.998116453123232));
#9952=CARTESIAN_POINT('Ctrl Pts',(0.032461919069828,-0.378143583103513,
-0.999591823858855));
#9953=CARTESIAN_POINT('Ctrl Pts',(0.0157128711428662,-0.375,-1.));
#9954=CARTESIAN_POINT('Ctrl Pts',(3.81639164714898E-17,-0.375,-1.));
#9955=CARTESIAN_POINT('',(-0.125,-0.5,-0.992156741649222));
#9956=CARTESIAN_POINT('Ctrl Pts',(4.5102810375397E-17,-0.375,-1.));
#9957=CARTESIAN_POINT('Ctrl Pts',(-0.0157128711428661,-0.375,-1.));
#9958=CARTESIAN_POINT('Ctrl Pts',(-0.0324619190698279,-0.378143583103513,
-0.999591823858855));
#9959=CARTESIAN_POINT('Ctrl Pts',(-0.0632545375991437,-0.390905426591754,
-0.998116453123232));
#9960=CARTESIAN_POINT('Ctrl Pts',(-0.0772994769543643,-0.400522781657727,
-0.997070068816062));
#9961=CARTESIAN_POINT('Ctrl Pts',(-0.099477310980424,-0.422700615683787,
-0.995102104277285));
#9962=CARTESIAN_POINT('Ctrl Pts',(-0.109094593469654,-0.436745514765346,
-0.994052129228928));
#9963=CARTESIAN_POINT('Ctrl Pts',(-0.121856383722779,-0.467537996927464,
-0.99256853061881));
#9964=CARTESIAN_POINT('Ctrl Pts',(-0.125,-0.484286997589363,-0.992156741649222));
#9965=CARTESIAN_POINT('Ctrl Pts',(-0.125,-0.5,-0.992156741649222));
#9966=CARTESIAN_POINT('Ctrl Pts',(-0.125,-0.5,-0.992156741649222));
#9967=CARTESIAN_POINT('Ctrl Pts',(-0.125,-0.515713002410637,-0.992156741649222));
#9968=CARTESIAN_POINT('Ctrl Pts',(-0.121856383722779,-0.532462003072536,
-0.99256853061881));
#9969=CARTESIAN_POINT('Ctrl Pts',(-0.109094593469654,-0.563254485234654,
-0.994052129228928));
#9970=CARTESIAN_POINT('Ctrl Pts',(-0.0994773109804241,-0.577299384316213,
-0.995102104277285));
#9971=CARTESIAN_POINT('Ctrl Pts',(-0.0772994769543644,-0.599477218342273,
-0.997070068816062));
#9972=CARTESIAN_POINT('Ctrl Pts',(-0.0632545375991439,-0.609094573408246,
-0.998116453123232));
#9973=CARTESIAN_POINT('Ctrl Pts',(-0.032461919069828,-0.621856416896487,
-0.999591823858855));
#9974=CARTESIAN_POINT('Ctrl Pts',(-0.0157128711428662,-0.625,-1.));
#9975=CARTESIAN_POINT('Ctrl Pts',(-1.38777878078145E-17,-0.625,-1.));
#9976=CARTESIAN_POINT('',(0.,-0.375,1.));
#9977=CARTESIAN_POINT('',(0.,-0.625,1.));
#9978=CARTESIAN_POINT('Ctrl Pts',(4.16333634234434E-17,-0.375,1.));
#9979=CARTESIAN_POINT('Ctrl Pts',(0.0157128711428662,-0.375,1.));
#9980=CARTESIAN_POINT('Ctrl Pts',(0.032461919069828,-0.378143583103513,
0.999591823858855));
#9981=CARTESIAN_POINT('Ctrl Pts',(0.0632545375991439,-0.390905426591754,
0.998116453123232));
#9982=CARTESIAN_POINT('Ctrl Pts',(0.0772994769543644,-0.400522781657728,
0.997070068816062));
#9983=CARTESIAN_POINT('Ctrl Pts',(0.0994773109804241,-0.422700615683787,
0.995102104277285));
#9984=CARTESIAN_POINT('Ctrl Pts',(0.109094593469654,-0.436745514765346,
0.994052129228928));
#9985=CARTESIAN_POINT('Ctrl Pts',(0.121856383722779,-0.467537996927464,
0.99256853061881));
#9986=CARTESIAN_POINT('Ctrl Pts',(0.125,-0.484286997589363,0.992156741649222));
#9987=CARTESIAN_POINT('Ctrl Pts',(0.125,-0.515713002410637,0.992156741649222));
#9988=CARTESIAN_POINT('Ctrl Pts',(0.121856383722779,-0.532462003072536,
0.99256853061881));
#9989=CARTESIAN_POINT('Ctrl Pts',(0.109094593469655,-0.563254485234654,
0.994052129228928));
#9990=CARTESIAN_POINT('Ctrl Pts',(0.0994773109804241,-0.577299384316213,
0.995102104277285));
#9991=CARTESIAN_POINT('Ctrl Pts',(0.0772994769543644,-0.599477218342273,
0.997070068816062));
#9992=CARTESIAN_POINT('Ctrl Pts',(0.0632545375991438,-0.609094573408246,
0.998116453123232));
#9993=CARTESIAN_POINT('Ctrl Pts',(0.0324619190698279,-0.621856416896487,
0.999591823858855));
#9994=CARTESIAN_POINT('Ctrl Pts',(0.0157128711428662,-0.625,1.));
#9995=CARTESIAN_POINT('Ctrl Pts',(-1.73472347597681E-17,-0.625,1.));
#9996=CARTESIAN_POINT('',(-0.125,-0.5,0.992156741649222));
#9997=CARTESIAN_POINT('Ctrl Pts',(-1.73472347597681E-17,-0.625,1.));
#9998=CARTESIAN_POINT('Ctrl Pts',(-0.0157128711428662,-0.625,1.));
#9999=CARTESIAN_POINT('Ctrl Pts',(-0.032461919069828,-0.621856416896487,
0.999591823858855));
#10000=CARTESIAN_POINT('Ctrl Pts',(-0.0632545375991439,-0.609094573408246,
0.998116453123232));
#10001=CARTESIAN_POINT('Ctrl Pts',(-0.0772994769543645,-0.599477218342273,
0.997070068816062));
#10002=CARTESIAN_POINT('Ctrl Pts',(-0.0994773109804241,-0.577299384316213,
0.995102104277285));
#10003=CARTESIAN_POINT('Ctrl Pts',(-0.109094593469654,-0.563254485234654,
0.994052129228928));
#10004=CARTESIAN_POINT('Ctrl Pts',(-0.121856383722779,-0.532462003072536,
0.99256853061881));
#10005=CARTESIAN_POINT('Ctrl Pts',(-0.125,-0.515713002410637,0.992156741649222));
#10006=CARTESIAN_POINT('Ctrl Pts',(-0.125,-0.5,0.992156741649222));
#10007=CARTESIAN_POINT('Ctrl Pts',(-0.125,-0.5,0.992156741649222));
#10008=CARTESIAN_POINT('Ctrl Pts',(-0.125,-0.484286997589363,0.992156741649222));
#10009=CARTESIAN_POINT('Ctrl Pts',(-0.121856383722779,-0.467537996927464,
0.99256853061881));
#10010=CARTESIAN_POINT('Ctrl Pts',(-0.109094593469654,-0.436745514765346,
0.994052129228928));
#10011=CARTESIAN_POINT('Ctrl Pts',(-0.099477310980424,-0.422700615683787,
0.995102104277285));
#10012=CARTESIAN_POINT('Ctrl Pts',(-0.0772994769543643,-0.400522781657727,
0.997070068816062));
#10013=CARTESIAN_POINT('Ctrl Pts',(-0.0632545375991438,-0.390905426591754,
0.998116453123232));
#10014=CARTESIAN_POINT('Ctrl Pts',(-0.0324619190698279,-0.378143583103513,
0.999591823858855));
#10015=CARTESIAN_POINT('Ctrl Pts',(-0.0157128711428661,-0.375,1.));
#10016=CARTESIAN_POINT('Ctrl Pts',(4.5102810375397E-17,-0.375,1.));
#10017=CARTESIAN_POINT('Origin',(0.,-0.5,0.));
#10018=CARTESIAN_POINT('',(-0.125,-0.5,0.));
#10019=CARTESIAN_POINT('Origin',(0.,-0.5,0.));
#10020=CARTESIAN_POINT('',(-0.125,-0.5,0.));
#10021=CARTESIAN_POINT('Origin',(0.,-0.9,0.));
#10022=CARTESIAN_POINT('Origin',(0.,0.,0.));
#10023=CARTESIAN_POINT('',(-1.4,0.,1.71450551880629E-16));
#10024=CARTESIAN_POINT('Origin',(0.,0.,0.));
#10025=CARTESIAN_POINT('',(1.23958209161204,0.,0.143317017690053));
#10026=CARTESIAN_POINT('',(1.22320001975977,0.,0.246749348660852));
#10027=CARTESIAN_POINT('Origin',(1.21321664662686,0.,0.192154639568406));
#10028=CARTESIAN_POINT('',(1.20190105810224,0.,0.335465908756113));
#10029=CARTESIAN_POINT('Origin',(0.,0.,0.));
#10030=CARTESIAN_POINT('',(1.16954029537568,0.,0.435062095450087));
#10031=CARTESIAN_POINT('Origin',(1.1682203282434,0.,0.379577794185952));
#10032=CARTESIAN_POINT('',(1.13462523166105,0.,0.519354515801077));
#10033=CARTESIAN_POINT('Origin',(0.,0.,0.));
#10034=CARTESIAN_POINT('',(1.08708260743774,0.,0.612662169561029));
#10035=CARTESIAN_POINT('Origin',(1.0944585482776,0.,0.557654483764164));
#10036=CARTESIAN_POINT('',(1.0394111664111,0.,0.690454891028201));
#10037=CARTESIAN_POINT('Origin',(0.,0.,0.));
#10038=CARTESIAN_POINT('',(0.977857337884349,0.,0.775176467748211));
#10039=CARTESIAN_POINT('Origin',(0.993747566553533,0.,0.72199986920298));
#10040=CARTESIAN_POINT('',(0.918603348636233,0.,0.844553975349804));
#10041=CARTESIAN_POINT('Origin',(0.,0.,0.));
#10042=CARTESIAN_POINT('',(0.844553975349804,0.,0.918603348636233));
#10043=CARTESIAN_POINT('Origin',(0.86856722168183,0.,0.86856722168183));
#10044=CARTESIAN_POINT('',(0.775176467748211,0.,0.977857337884349));
#10045=CARTESIAN_POINT('Origin',(0.,0.,0.));
#10046=CARTESIAN_POINT('',(0.690454891028201,0.,1.0394111664111));
#10047=CARTESIAN_POINT('Origin',(0.721999869202979,0.,0.993747566553533));
#10048=CARTESIAN_POINT('',(0.612662169561028,0.,1.08708260743774));
#10049=CARTESIAN_POINT('Origin',(0.,0.,0.));
#10050=CARTESIAN_POINT('',(0.519354515801077,0.,1.13462523166105));
#10051=CARTESIAN_POINT('Origin',(0.557654483764164,0.,1.0944585482776));
#10052=CARTESIAN_POINT('',(0.435062095450087,0.,1.16954029537568));
#10053=CARTESIAN_POINT('Origin',(0.,0.,0.));
#10054=CARTESIAN_POINT('',(0.335465908756113,0.,1.20190105810224));
#10055=CARTESIAN_POINT('Origin',(0.379577794185951,0.,1.1682203282434));
#10056=CARTESIAN_POINT('',(0.246749348660851,0.,1.22320001975977));
#10057=CARTESIAN_POINT('Origin',(0.,0.,0.));
#10058=CARTESIAN_POINT('',(0.143317017690053,0.,1.23958209161204));
#10059=CARTESIAN_POINT('Origin',(0.192154639568406,0.,1.21321664662686));
#10060=CARTESIAN_POINT('',(0.0523608139934478,0.,1.24674050008925));
#10061=CARTESIAN_POINT('Origin',(0.,0.,0.));
#10062=CARTESIAN_POINT('',(-0.0523608139934483,0.,1.24674050008925));
#10063=CARTESIAN_POINT('Origin',(-2.25642313758905E-16,0.,1.22833954473516));
#10064=CARTESIAN_POINT('',(-0.143317017690053,0.,1.23958209161204));
#10065=CARTESIAN_POINT('Origin',(0.,0.,0.));
#10066=CARTESIAN_POINT('',(-0.246749348660852,0.,1.22320001975977));
#10067=CARTESIAN_POINT('Origin',(-0.192154639568406,0.,1.21321664662686));
#10068=CARTESIAN_POINT('',(-0.335465908756113,0.,1.20190105810224));
#10069=CARTESIAN_POINT('Origin',(0.,0.,0.));
#10070=CARTESIAN_POINT('',(-0.435062095450087,0.,1.16954029537568));
#10071=CARTESIAN_POINT('Origin',(-0.379577794185951,0.,1.1682203282434));
#10072=CARTESIAN_POINT('',(-0.519354515801077,0.,1.13462523166105));
#10073=CARTESIAN_POINT('Origin',(0.,0.,0.));
#10074=CARTESIAN_POINT('',(-0.612662169561029,0.,1.08708260743774));
#10075=CARTESIAN_POINT('Origin',(-0.557654483764164,0.,1.0944585482776));
#10076=CARTESIAN_POINT('',(-0.690454891028201,0.,1.0394111664111));
#10077=CARTESIAN_POINT('Origin',(0.,0.,0.));
#10078=CARTESIAN_POINT('',(-0.775176467748211,0.,0.977857337884349));
#10079=CARTESIAN_POINT('Origin',(-0.721999869202979,0.,0.993747566553533));
#10080=CARTESIAN_POINT('',(-0.844553975349804,0.,0.918603348636233));
#10081=CARTESIAN_POINT('Origin',(0.,0.,0.));
#10082=CARTESIAN_POINT('',(-0.918603348636233,0.,0.844553975349804));
#10083=CARTESIAN_POINT('Origin',(-0.86856722168183,0.,0.86856722168183));
#10084=CARTESIAN_POINT('',(-0.977857337884348,0.,0.775176467748211));
#10085=CARTESIAN_POINT('Origin',(0.,0.,0.));
#10086=CARTESIAN_POINT('',(-1.0394111664111,0.,0.690454891028201));
#10087=CARTESIAN_POINT('Origin',(-0.993747566553533,0.,0.721999869202979));
#10088=CARTESIAN_POINT('',(-1.08708260743774,0.,0.612662169561028));
#10089=CARTESIAN_POINT('Origin',(0.,0.,0.));
#10090=CARTESIAN_POINT('',(-1.13462523166105,0.,0.519354515801077));
#10091=CARTESIAN_POINT('Origin',(-1.0944585482776,0.,0.557654483764164));
#10092=CARTESIAN_POINT('',(-1.16954029537568,0.,0.435062095450087));
#10093=CARTESIAN_POINT('Origin',(0.,0.,0.));
#10094=CARTESIAN_POINT('',(-1.20190105810224,0.,0.335465908756113));
#10095=CARTESIAN_POINT('Origin',(-1.1682203282434,0.,0.379577794185951));
#10096=CARTESIAN_POINT('',(-1.22320001975977,0.,0.246749348660851));
#10097=CARTESIAN_POINT('Origin',(0.,0.,0.));
#10098=CARTESIAN_POINT('',(-1.23958209161204,0.,0.143317017690053));
#10099=CARTESIAN_POINT('Origin',(-1.21321664662686,0.,0.192154639568406));
#10100=CARTESIAN_POINT('',(-1.24674050008925,0.,0.0523608139934479));
#10101=CARTESIAN_POINT('Origin',(0.,0.,0.));
#10102=CARTESIAN_POINT('',(-1.24674050008925,0.,-0.0523608139934482));
#10103=CARTESIAN_POINT('Origin',(-1.22833954473516,0.,-1.50428209172603E-16));
#10104=CARTESIAN_POINT('',(-1.23958209161204,0.,-0.143317017690053));
#10105=CARTESIAN_POINT('Origin',(0.,0.,0.));
#10106=CARTESIAN_POINT('',(-1.22320001975977,0.,-0.246749348660852));
#10107=CARTESIAN_POINT('Origin',(-1.21321664662686,0.,-0.192154639568406));
#10108=CARTESIAN_POINT('',(-1.20190105810224,0.,-0.335465908756113));
#10109=CARTESIAN_POINT('Origin',(0.,0.,0.));
#10110=CARTESIAN_POINT('',(-1.16954029537568,0.,-0.435062095450087));
#10111=CARTESIAN_POINT('Origin',(-1.1682203282434,0.,-0.379577794185951));
#10112=CARTESIAN_POINT('',(-1.13462523166105,0.,-0.519354515801077));
#10113=CARTESIAN_POINT('Origin',(0.,0.,0.));
#10114=CARTESIAN_POINT('',(-1.08708260743774,0.,-0.612662169561029));
#10115=CARTESIAN_POINT('Origin',(-1.0944585482776,0.,-0.557654483764164));
#10116=CARTESIAN_POINT('',(-1.0394111664111,0.,-0.690454891028201));
#10117=CARTESIAN_POINT('Origin',(0.,0.,0.));
#10118=CARTESIAN_POINT('',(-0.977857337884349,0.,-0.775176467748211));
#10119=CARTESIAN_POINT('Origin',(-0.993747566553533,0.,-0.721999869202979));
#10120=CARTESIAN_POINT('',(-0.918603348636233,0.,-0.844553975349804));
#10121=CARTESIAN_POINT('Origin',(0.,0.,0.));
#10122=CARTESIAN_POINT('',(-0.844553975349804,0.,-0.918603348636233));
#10123=CARTESIAN_POINT('Origin',(-0.86856722168183,0.,-0.86856722168183));
#10124=CARTESIAN_POINT('',(-0.775176467748211,0.,-0.977857337884348));
#10125=CARTESIAN_POINT('Origin',(0.,0.,0.));
#10126=CARTESIAN_POINT('',(-0.690454891028201,0.,-1.0394111664111));
#10127=CARTESIAN_POINT('Origin',(-0.721999869202979,0.,-0.993747566553533));
#10128=CARTESIAN_POINT('',(-0.612662169561028,0.,-1.08708260743774));
#10129=CARTESIAN_POINT('Origin',(0.,0.,0.));
#10130=CARTESIAN_POINT('',(-0.519354515801077,0.,-1.13462523166105));
#10131=CARTESIAN_POINT('Origin',(-0.557654483764164,0.,-1.0944585482776));
#10132=CARTESIAN_POINT('',(-0.435062095450087,0.,-1.16954029537568));
#10133=CARTESIAN_POINT('Origin',(0.,0.,0.));
#10134=CARTESIAN_POINT('',(-0.335465908756113,0.,-1.20190105810224));
#10135=CARTESIAN_POINT('Origin',(-0.379577794185951,0.,-1.1682203282434));
#10136=CARTESIAN_POINT('',(-0.246749348660852,0.,-1.22320001975977));
#10137=CARTESIAN_POINT('Origin',(0.,0.,0.));
#10138=CARTESIAN_POINT('',(-0.143317017690053,0.,-1.23958209161204));
#10139=CARTESIAN_POINT('Origin',(-0.192154639568406,0.,-1.21321664662686));
#10140=CARTESIAN_POINT('',(-0.0523608139934479,0.,-1.24674050008925));
#10141=CARTESIAN_POINT('Origin',(0.,0.,0.));
#10142=CARTESIAN_POINT('',(0.0523608139934481,0.,-1.24674050008925));
#10143=CARTESIAN_POINT('Origin',(7.52141045863017E-17,0.,-1.22833954473516));
#10144=CARTESIAN_POINT('',(0.143317017690053,0.,-1.23958209161204));
#10145=CARTESIAN_POINT('Origin',(0.,0.,0.));
#10146=CARTESIAN_POINT('',(0.246749348660852,0.,-1.22320001975977));
#10147=CARTESIAN_POINT('Origin',(0.192154639568406,0.,-1.21321664662686));
#10148=CARTESIAN_POINT('',(0.335465908756113,0.,-1.20190105810224));
#10149=CARTESIAN_POINT('Origin',(0.,0.,0.));
#10150=CARTESIAN_POINT('',(0.435062095450087,0.,-1.16954029537568));
#10151=CARTESIAN_POINT('Origin',(0.379577794185951,0.,-1.1682203282434));
#10152=CARTESIAN_POINT('',(0.519354515801077,0.,-1.13462523166105));
#10153=CARTESIAN_POINT('Origin',(0.,0.,0.));
#10154=CARTESIAN_POINT('',(0.612662169561028,0.,-1.08708260743774));
#10155=CARTESIAN_POINT('Origin',(0.557654483764164,0.,-1.0944585482776));
#10156=CARTESIAN_POINT('',(0.690454891028201,0.,-1.0394111664111));
#10157=CARTESIAN_POINT('Origin',(0.,0.,0.));
#10158=CARTESIAN_POINT('',(0.775176467748211,0.,-0.977857337884349));
#10159=CARTESIAN_POINT('Origin',(0.721999869202979,0.,-0.993747566553533));
#10160=CARTESIAN_POINT('',(0.844553975349804,0.,-0.918603348636233));
#10161=CARTESIAN_POINT('Origin',(0.,0.,0.));
#10162=CARTESIAN_POINT('',(0.918603348636233,0.,-0.844553975349804));
#10163=CARTESIAN_POINT('Origin',(0.86856722168183,0.,-0.86856722168183));
#10164=CARTESIAN_POINT('',(0.977857337884349,0.,-0.775176467748211));
#10165=CARTESIAN_POINT('Origin',(0.,0.,0.));
#10166=CARTESIAN_POINT('',(1.0394111664111,0.,-0.690454891028201));
#10167=CARTESIAN_POINT('Origin',(0.993747566553533,0.,-0.721999869202979));
#10168=CARTESIAN_POINT('',(1.08708260743774,0.,-0.612662169561028));
#10169=CARTESIAN_POINT('Origin',(0.,0.,0.));
#10170=CARTESIAN_POINT('',(1.13462523166105,0.,-0.519354515801077));
#10171=CARTESIAN_POINT('Origin',(1.0944585482776,0.,-0.557654483764164));
#10172=CARTESIAN_POINT('',(1.16954029537568,0.,-0.43506209545009));
#10173=CARTESIAN_POINT('Origin',(0.,0.,0.));
#10174=CARTESIAN_POINT('',(1.20190105810224,0.,-0.33546590875611));
#10175=CARTESIAN_POINT('Origin',(1.1682203282434,0.,-0.379577794185951));
#10176=CARTESIAN_POINT('',(1.22320001975977,0.,-0.246749348660852));
#10177=CARTESIAN_POINT('Origin',(0.,0.,0.));
#10178=CARTESIAN_POINT('',(1.23958209161204,0.,-0.143317017690053));
#10179=CARTESIAN_POINT('Origin',(1.21321664662686,0.,-0.192154639568406));
#10180=CARTESIAN_POINT('',(1.24674050008925,0.,-0.052360813993451));
#10181=CARTESIAN_POINT('Origin',(0.,0.,0.));
#10182=CARTESIAN_POINT('',(1.24674050008925,0.,0.052360813993451));
#10183=CARTESIAN_POINT('Origin',(1.22833954473516,0.,0.));
#10184=CARTESIAN_POINT('Origin',(0.,0.,0.));
#10185=CARTESIAN_POINT('Origin',(0.,0.,0.));
#10186=CARTESIAN_POINT('',(-1.4,-0.1,1.71450551880629E-16));
#10187=CARTESIAN_POINT('Origin',(0.,-0.1,0.));
#10188=CARTESIAN_POINT('',(-1.4,0.,-1.71450551880629E-16));
#10189=CARTESIAN_POINT('Origin',(0.,-0.1,0.));
#10190=CARTESIAN_POINT('Origin',(0.,0.75,0.));
#10191=CARTESIAN_POINT('',(-1.4,0.75,1.71450551880629E-16));
#10192=CARTESIAN_POINT('Origin',(0.,0.75,0.));
#10193=CARTESIAN_POINT('',(1.22320001975977,0.75,0.246749348660852));
#10194=CARTESIAN_POINT('',(1.23958209161204,0.75,0.143317017690053));
#10195=CARTESIAN_POINT('Origin',(1.21321664662686,0.75,0.192154639568406));
#10196=CARTESIAN_POINT('',(1.24674050008925,0.75,0.052360813993448));
#10197=CARTESIAN_POINT('Origin',(0.,0.75,0.));
#10198=CARTESIAN_POINT('',(1.24674050008925,0.75,-0.052360813993448));
#10199=CARTESIAN_POINT('Origin',(1.22833954473516,0.75,0.));
#10200=CARTESIAN_POINT('',(1.23958209161204,0.75,-0.143317017690053));
#10201=CARTESIAN_POINT('Origin',(0.,0.75,0.));
#10202=CARTESIAN_POINT('',(1.22320001975977,0.75,-0.246749348660852));
#10203=CARTESIAN_POINT('Origin',(1.21321664662686,0.75,-0.192154639568406));
#10204=CARTESIAN_POINT('',(1.20190105810224,0.75,-0.335465908756113));
#10205=CARTESIAN_POINT('Origin',(0.,0.75,0.));
#10206=CARTESIAN_POINT('',(1.16954029537568,0.75,-0.435062095450087));
#10207=CARTESIAN_POINT('Origin',(1.1682203282434,0.75,-0.379577794185951));
#10208=CARTESIAN_POINT('',(1.13462523166105,0.75,-0.519354515801077));
#10209=CARTESIAN_POINT('Origin',(0.,0.75,0.));
#10210=CARTESIAN_POINT('',(1.08708260743774,0.75,-0.612662169561028));
#10211=CARTESIAN_POINT('Origin',(1.0944585482776,0.75,-0.557654483764164));
#10212=CARTESIAN_POINT('',(1.0394111664111,0.75,-0.690454891028201));
#10213=CARTESIAN_POINT('Origin',(0.,0.75,0.));
#10214=CARTESIAN_POINT('',(0.977857337884349,0.75,-0.775176467748211));
#10215=CARTESIAN_POINT('Origin',(0.993747566553533,0.75,-0.721999869202979));
#10216=CARTESIAN_POINT('',(0.918603348636233,0.75,-0.844553975349804));
#10217=CARTESIAN_POINT('Origin',(0.,0.75,0.));
#10218=CARTESIAN_POINT('',(0.844553975349804,0.75,-0.918603348636233));
#10219=CARTESIAN_POINT('Origin',(0.86856722168183,0.75,-0.86856722168183));
#10220=CARTESIAN_POINT('',(0.775176467748211,0.75,-0.977857337884349));
#10221=CARTESIAN_POINT('Origin',(0.,0.75,0.));
#10222=CARTESIAN_POINT('',(0.690454891028201,0.75,-1.0394111664111));
#10223=CARTESIAN_POINT('Origin',(0.721999869202979,0.75,-0.993747566553533));
#10224=CARTESIAN_POINT('',(0.612662169561028,0.75,-1.08708260743774));
#10225=CARTESIAN_POINT('Origin',(0.,0.75,0.));
#10226=CARTESIAN_POINT('',(0.519354515801077,0.75,-1.13462523166105));
#10227=CARTESIAN_POINT('Origin',(0.557654483764164,0.75,-1.0944585482776));
#10228=CARTESIAN_POINT('',(0.435062095450087,0.75,-1.16954029537568));
#10229=CARTESIAN_POINT('Origin',(0.,0.75,0.));
#10230=CARTESIAN_POINT('',(0.335465908756113,0.75,-1.20190105810224));
#10231=CARTESIAN_POINT('Origin',(0.379577794185951,0.75,-1.1682203282434));
#10232=CARTESIAN_POINT('',(0.246749348660852,0.75,-1.22320001975977));
#10233=CARTESIAN_POINT('Origin',(0.,0.75,0.));
#10234=CARTESIAN_POINT('',(0.143317017690053,0.75,-1.23958209161204));
#10235=CARTESIAN_POINT('Origin',(0.192154639568406,0.75,-1.21321664662686));
#10236=CARTESIAN_POINT('',(0.0523608139934481,0.75,-1.24674050008925));
#10237=CARTESIAN_POINT('Origin',(0.,0.75,0.));
#10238=CARTESIAN_POINT('',(-0.0523608139934479,0.75,-1.24674050008925));
#10239=CARTESIAN_POINT('Origin',(7.52141045863017E-17,0.75,-1.22833954473516));
#10240=CARTESIAN_POINT('',(-0.143317017690053,0.75,-1.23958209161204));
#10241=CARTESIAN_POINT('Origin',(0.,0.75,0.));
#10242=CARTESIAN_POINT('',(-0.246749348660852,0.75,-1.22320001975977));
#10243=CARTESIAN_POINT('Origin',(-0.192154639568406,0.75,-1.21321664662686));
#10244=CARTESIAN_POINT('',(-0.335465908756113,0.75,-1.20190105810224));
#10245=CARTESIAN_POINT('Origin',(0.,0.75,0.));
#10246=CARTESIAN_POINT('',(-0.435062095450087,0.75,-1.16954029537568));
#10247=CARTESIAN_POINT('Origin',(-0.379577794185951,0.75,-1.1682203282434));
#10248=CARTESIAN_POINT('',(-0.519354515801077,0.75,-1.13462523166105));
#10249=CARTESIAN_POINT('Origin',(0.,0.75,0.));
#10250=CARTESIAN_POINT('',(-0.612662169561028,0.75,-1.08708260743774));
#10251=CARTESIAN_POINT('Origin',(-0.557654483764164,0.75,-1.0944585482776));
#10252=CARTESIAN_POINT('',(-0.690454891028201,0.75,-1.0394111664111));
#10253=CARTESIAN_POINT('Origin',(0.,0.75,0.));
#10254=CARTESIAN_POINT('',(-0.775176467748211,0.75,-0.977857337884348));
#10255=CARTESIAN_POINT('Origin',(-0.721999869202979,0.75,-0.993747566553533));
#10256=CARTESIAN_POINT('',(-0.844553975349804,0.75,-0.918603348636233));
#10257=CARTESIAN_POINT('Origin',(0.,0.75,0.));
#10258=CARTESIAN_POINT('',(-0.918603348636233,0.75,-0.844553975349804));
#10259=CARTESIAN_POINT('Origin',(-0.86856722168183,0.75,-0.86856722168183));
#10260=CARTESIAN_POINT('',(-0.977857337884349,0.75,-0.775176467748211));
#10261=CARTESIAN_POINT('Origin',(0.,0.75,0.));
#10262=CARTESIAN_POINT('',(-1.0394111664111,0.75,-0.690454891028201));
#10263=CARTESIAN_POINT('Origin',(-0.993747566553533,0.75,-0.721999869202979));
#10264=CARTESIAN_POINT('',(-1.08708260743774,0.75,-0.612662169561029));
#10265=CARTESIAN_POINT('Origin',(0.,0.75,0.));
#10266=CARTESIAN_POINT('',(-1.13462523166105,0.75,-0.519354515801077));
#10267=CARTESIAN_POINT('Origin',(-1.0944585482776,0.75,-0.557654483764164));
#10268=CARTESIAN_POINT('',(-1.16954029537568,0.75,-0.435062095450087));
#10269=CARTESIAN_POINT('Origin',(0.,0.75,0.));
#10270=CARTESIAN_POINT('',(-1.20190105810224,0.75,-0.335465908756113));
#10271=CARTESIAN_POINT('Origin',(-1.1682203282434,0.75,-0.379577794185951));
#10272=CARTESIAN_POINT('',(-1.22320001975977,0.75,-0.246749348660852));
#10273=CARTESIAN_POINT('Origin',(0.,0.75,0.));
#10274=CARTESIAN_POINT('',(-1.23958209161204,0.75,-0.143317017690053));
#10275=CARTESIAN_POINT('Origin',(-1.21321664662686,0.75,-0.192154639568406));
#10276=CARTESIAN_POINT('',(-1.24674050008925,0.75,-0.0523608139934482));
#10277=CARTESIAN_POINT('Origin',(0.,0.75,0.));
#10278=CARTESIAN_POINT('',(-1.24674050008925,0.75,0.0523608139934479));
#10279=CARTESIAN_POINT('Origin',(-1.22833954473516,0.75,-1.50428209172603E-16));
#10280=CARTESIAN_POINT('',(-1.23958209161204,0.75,0.143317017690053));
#10281=CARTESIAN_POINT('Origin',(0.,0.75,0.));
#10282=CARTESIAN_POINT('',(-1.22320001975977,0.75,0.246749348660851));
#10283=CARTESIAN_POINT('Origin',(-1.21321664662686,0.75,0.192154639568406));
#10284=CARTESIAN_POINT('',(-1.20190105810224,0.75,0.335465908756113));
#10285=CARTESIAN_POINT('Origin',(0.,0.75,0.));
#10286=CARTESIAN_POINT('',(-1.16954029537568,0.75,0.435062095450087));
#10287=CARTESIAN_POINT('Origin',(-1.1682203282434,0.75,0.379577794185951));
#10288=CARTESIAN_POINT('',(-1.13462523166105,0.75,0.519354515801077));
#10289=CARTESIAN_POINT('Origin',(0.,0.75,0.));
#10290=CARTESIAN_POINT('',(-1.08708260743774,0.75,0.612662169561028));
#10291=CARTESIAN_POINT('Origin',(-1.0944585482776,0.75,0.557654483764164));
#10292=CARTESIAN_POINT('',(-1.0394111664111,0.75,0.690454891028201));
#10293=CARTESIAN_POINT('Origin',(0.,0.75,0.));
#10294=CARTESIAN_POINT('',(-0.977857337884348,0.75,0.775176467748211));
#10295=CARTESIAN_POINT('Origin',(-0.993747566553533,0.75,0.721999869202979));
#10296=CARTESIAN_POINT('',(-0.918603348636233,0.75,0.844553975349804));
#10297=CARTESIAN_POINT('Origin',(0.,0.75,0.));
#10298=CARTESIAN_POINT('',(-0.844553975349804,0.75,0.918603348636233));
#10299=CARTESIAN_POINT('Origin',(-0.86856722168183,0.75,0.86856722168183));
#10300=CARTESIAN_POINT('',(-0.775176467748211,0.75,0.977857337884349));
#10301=CARTESIAN_POINT('Origin',(0.,0.75,0.));
#10302=CARTESIAN_POINT('',(-0.690454891028201,0.75,1.0394111664111));
#10303=CARTESIAN_POINT('Origin',(-0.721999869202979,0.75,0.993747566553533));
#10304=CARTESIAN_POINT('',(-0.612662169561029,0.75,1.08708260743774));
#10305=CARTESIAN_POINT('Origin',(0.,0.75,0.));
#10306=CARTESIAN_POINT('',(-0.519354515801077,0.75,1.13462523166105));
#10307=CARTESIAN_POINT('Origin',(-0.557654483764164,0.75,1.0944585482776));
#10308=CARTESIAN_POINT('',(-0.435062095450087,0.75,1.16954029537568));
#10309=CARTESIAN_POINT('Origin',(0.,0.75,0.));
#10310=CARTESIAN_POINT('',(-0.335465908756113,0.75,1.20190105810224));
#10311=CARTESIAN_POINT('Origin',(-0.379577794185951,0.75,1.1682203282434));
#10312=CARTESIAN_POINT('',(-0.246749348660852,0.75,1.22320001975977));
#10313=CARTESIAN_POINT('Origin',(0.,0.75,0.));
#10314=CARTESIAN_POINT('',(-0.143317017690053,0.75,1.23958209161204));
#10315=CARTESIAN_POINT('Origin',(-0.192154639568406,0.75,1.21321664662686));
#10316=CARTESIAN_POINT('',(-0.0523608139934483,0.75,1.24674050008925));
#10317=CARTESIAN_POINT('Origin',(0.,0.75,0.));
#10318=CARTESIAN_POINT('',(0.0523608139934478,0.75,1.24674050008925));
#10319=CARTESIAN_POINT('Origin',(-2.25642313758905E-16,0.75,1.22833954473516));
#10320=CARTESIAN_POINT('',(0.143317017690053,0.75,1.23958209161204));
#10321=CARTESIAN_POINT('Origin',(0.,0.75,0.));
#10322=CARTESIAN_POINT('',(0.246749348660851,0.75,1.22320001975977));
#10323=CARTESIAN_POINT('Origin',(0.192154639568406,0.75,1.21321664662686));
#10324=CARTESIAN_POINT('',(0.335465908756113,0.75,1.20190105810224));
#10325=CARTESIAN_POINT('Origin',(0.,0.75,0.));
#10326=CARTESIAN_POINT('',(0.435062095450087,0.75,1.16954029537568));
#10327=CARTESIAN_POINT('Origin',(0.379577794185951,0.75,1.1682203282434));
#10328=CARTESIAN_POINT('',(0.519354515801077,0.75,1.13462523166105));
#10329=CARTESIAN_POINT('Origin',(0.,0.75,0.));
#10330=CARTESIAN_POINT('',(0.612662169561028,0.75,1.08708260743774));
#10331=CARTESIAN_POINT('Origin',(0.557654483764164,0.75,1.0944585482776));
#10332=CARTESIAN_POINT('',(0.690454891028201,0.75,1.0394111664111));
#10333=CARTESIAN_POINT('Origin',(0.,0.75,0.));
#10334=CARTESIAN_POINT('',(0.775176467748211,0.75,0.977857337884349));
#10335=CARTESIAN_POINT('Origin',(0.721999869202979,0.75,0.993747566553533));
#10336=CARTESIAN_POINT('',(0.844553975349804,0.75,0.918603348636233));
#10337=CARTESIAN_POINT('Origin',(0.,0.75,0.));
#10338=CARTESIAN_POINT('',(0.918603348636233,0.75,0.844553975349804));
#10339=CARTESIAN_POINT('Origin',(0.86856722168183,0.75,0.86856722168183));
#10340=CARTESIAN_POINT('',(0.977857337884349,0.75,0.775176467748211));
#10341=CARTESIAN_POINT('Origin',(0.,0.75,0.));
#10342=CARTESIAN_POINT('',(1.0394111664111,0.75,0.690454891028201));
#10343=CARTESIAN_POINT('Origin',(0.993747566553533,0.75,0.72199986920298));
#10344=CARTESIAN_POINT('',(1.08708260743774,0.75,0.612662169561029));
#10345=CARTESIAN_POINT('Origin',(0.,0.75,0.));
#10346=CARTESIAN_POINT('',(1.13462523166105,0.75,0.519354515801077));
#10347=CARTESIAN_POINT('Origin',(1.0944585482776,0.75,0.557654483764164));
#10348=CARTESIAN_POINT('',(1.16954029537568,0.75,0.435062095450087));
#10349=CARTESIAN_POINT('Origin',(0.,0.75,0.));
#10350=CARTESIAN_POINT('',(1.20190105810224,0.75,0.335465908756113));
#10351=CARTESIAN_POINT('Origin',(1.1682203282434,0.75,0.379577794185952));
#10352=CARTESIAN_POINT('Origin',(0.,0.75,0.));
#10353=CARTESIAN_POINT('Origin',(0.,0.75,0.));
#10354=CARTESIAN_POINT('',(-1.4,0.75,1.71450551880629E-16));
#10355=CARTESIAN_POINT('Origin',(1.21321664662686,0.,0.192154639568406));
#10356=CARTESIAN_POINT('',(1.23958209161204,0.,0.14331701769005));
#10357=CARTESIAN_POINT('',(1.22320001975977,0.,0.246749348660855));
#10358=CARTESIAN_POINT('Origin',(0.,0.,0.));
#10359=CARTESIAN_POINT('',(1.20190105810224,0.,0.33546590875611));
#10360=CARTESIAN_POINT('Origin',(1.1682203282434,0.,0.379577794185952));
#10361=CARTESIAN_POINT('',(1.16954029537568,0.,0.43506209545009));
#10362=CARTESIAN_POINT('Origin',(0.,0.,0.));
#10363=CARTESIAN_POINT('',(1.13462523166105,0.,0.519354515801074));
#10364=CARTESIAN_POINT('Origin',(1.0944585482776,0.,0.557654483764164));
#10365=CARTESIAN_POINT('',(1.08708260743774,0.,0.612662169561031));
#10366=CARTESIAN_POINT('Origin',(0.,0.,0.));
#10367=CARTESIAN_POINT('',(1.03941116641111,0.,0.690454891028199));
#10368=CARTESIAN_POINT('Origin',(0.993747566553533,0.,0.72199986920298));
#10369=CARTESIAN_POINT('',(0.977857337884347,0.,0.775176467748214));
#10370=CARTESIAN_POINT('Origin',(0.,0.,0.));
#10371=CARTESIAN_POINT('',(0.918603348636235,0.,0.844553975349802));
#10372=CARTESIAN_POINT('Origin',(0.86856722168183,0.,0.86856722168183));
#10373=CARTESIAN_POINT('',(0.844553975349802,0.,0.918603348636235));
#10374=CARTESIAN_POINT('Origin',(0.,0.,0.));
#10375=CARTESIAN_POINT('',(0.775176467748213,0.,0.977857337884347));
#10376=CARTESIAN_POINT('Origin',(0.721999869202979,0.,0.993747566553533));
#10377=CARTESIAN_POINT('',(0.690454891028198,0.,1.03941116641111));
#10378=CARTESIAN_POINT('Origin',(0.,0.,0.));
#10379=CARTESIAN_POINT('',(0.612662169561031,0.,1.08708260743774));
#10380=CARTESIAN_POINT('Origin',(0.557654483764164,0.,1.0944585482776));
#10381=CARTESIAN_POINT('',(0.519354515801074,0.,1.13462523166105));
#10382=CARTESIAN_POINT('Origin',(0.,0.,0.));
#10383=CARTESIAN_POINT('',(0.43506209545009,0.,1.16954029537568));
#10384=CARTESIAN_POINT('Origin',(0.379577794185951,0.,1.1682203282434));
#10385=CARTESIAN_POINT('',(0.33546590875611,0.,1.20190105810224));
#10386=CARTESIAN_POINT('Origin',(0.,0.,0.));
#10387=CARTESIAN_POINT('',(0.246749348660854,0.,1.22320001975977));
#10388=CARTESIAN_POINT('Origin',(0.192154639568406,0.,1.21321664662686));
#10389=CARTESIAN_POINT('',(0.14331701769005,0.,1.23958209161204));
#10390=CARTESIAN_POINT('Origin',(0.,0.,0.));
#10391=CARTESIAN_POINT('',(0.0523608139934508,0.,1.24674050008925));
#10392=CARTESIAN_POINT('Origin',(-2.25642313758905E-16,0.,1.22833954473516));
#10393=CARTESIAN_POINT('',(-0.0523608139934513,0.,1.24674050008925));
#10394=CARTESIAN_POINT('Origin',(0.,0.,0.));
#10395=CARTESIAN_POINT('',(-0.14331701769005,0.,1.23958209161204));
#10396=CARTESIAN_POINT('Origin',(-0.192154639568406,0.,1.21321664662686));
#10397=CARTESIAN_POINT('',(-0.246749348660855,0.,1.22320001975977));
#10398=CARTESIAN_POINT('Origin',(0.,0.,0.));
#10399=CARTESIAN_POINT('',(-0.33546590875611,0.,1.20190105810224));
#10400=CARTESIAN_POINT('Origin',(-0.379577794185951,0.,1.1682203282434));
#10401=CARTESIAN_POINT('',(-0.43506209545009,0.,1.16954029537568));
#10402=CARTESIAN_POINT('Origin',(0.,0.,0.));
#10403=CARTESIAN_POINT('',(-0.519354515801074,0.,1.13462523166105));
#10404=CARTESIAN_POINT('Origin',(-0.557654483764164,0.,1.0944585482776));
#10405=CARTESIAN_POINT('',(-0.612662169561031,0.,1.08708260743774));
#10406=CARTESIAN_POINT('Origin',(0.,0.,0.));
#10407=CARTESIAN_POINT('',(-0.690454891028199,0.,1.03941116641111));
#10408=CARTESIAN_POINT('Origin',(-0.721999869202979,0.,0.993747566553533));
#10409=CARTESIAN_POINT('',(-0.775176467748213,0.,0.977857337884347));
#10410=CARTESIAN_POINT('Origin',(0.,0.,0.));
#10411=CARTESIAN_POINT('',(-0.844553975349802,0.,0.918603348636235));
#10412=CARTESIAN_POINT('Origin',(-0.86856722168183,0.,0.86856722168183));
#10413=CARTESIAN_POINT('',(-0.918603348636235,0.,0.844553975349802));
#10414=CARTESIAN_POINT('Origin',(0.,0.,0.));
#10415=CARTESIAN_POINT('',(-0.977857337884347,0.,0.775176467748213));
#10416=CARTESIAN_POINT('Origin',(-0.993747566553533,0.,0.721999869202979));
#10417=CARTESIAN_POINT('',(-1.03941116641111,0.,0.690454891028198));
#10418=CARTESIAN_POINT('Origin',(0.,0.,0.));
#10419=CARTESIAN_POINT('',(-1.08708260743774,0.,0.612662169561031));
#10420=CARTESIAN_POINT('Origin',(-1.0944585482776,0.,0.557654483764164));
#10421=CARTESIAN_POINT('',(-1.13462523166105,0.,0.519354515801074));
#10422=CARTESIAN_POINT('Origin',(0.,0.,0.));
#10423=CARTESIAN_POINT('',(-1.16954029537568,0.,0.43506209545009));
#10424=CARTESIAN_POINT('Origin',(-1.1682203282434,0.,0.379577794185951));
#10425=CARTESIAN_POINT('',(-1.20190105810224,0.,0.33546590875611));
#10426=CARTESIAN_POINT('Origin',(0.,0.,0.));
#10427=CARTESIAN_POINT('',(-1.22320001975977,0.,0.246749348660854));
#10428=CARTESIAN_POINT('Origin',(-1.21321664662686,0.,0.192154639568406));
#10429=CARTESIAN_POINT('',(-1.23958209161204,0.,0.14331701769005));
#10430=CARTESIAN_POINT('Origin',(0.,0.,0.));
#10431=CARTESIAN_POINT('',(-1.24674050008925,0.,0.0523608139934509));
#10432=CARTESIAN_POINT('Origin',(-1.22833954473516,0.,-1.50428209172603E-16));
#10433=CARTESIAN_POINT('',(-1.24674050008925,0.,-0.0523608139934512));
#10434=CARTESIAN_POINT('Origin',(0.,0.,0.));
#10435=CARTESIAN_POINT('',(-1.23958209161204,0.,-0.14331701769005));
#10436=CARTESIAN_POINT('Origin',(-1.21321664662686,0.,-0.192154639568406));
#10437=CARTESIAN_POINT('',(-1.22320001975977,0.,-0.246749348660855));
#10438=CARTESIAN_POINT('Origin',(0.,0.,0.));
#10439=CARTESIAN_POINT('',(-1.20190105810224,0.,-0.33546590875611));
#10440=CARTESIAN_POINT('Origin',(-1.1682203282434,0.,-0.379577794185951));
#10441=CARTESIAN_POINT('',(-1.16954029537568,0.,-0.43506209545009));
#10442=CARTESIAN_POINT('Origin',(0.,0.,0.));
#10443=CARTESIAN_POINT('',(-1.13462523166105,0.,-0.519354515801074));
#10444=CARTESIAN_POINT('Origin',(-1.0944585482776,0.,-0.557654483764164));
#10445=CARTESIAN_POINT('',(-1.08708260743774,0.,-0.612662169561031));
#10446=CARTESIAN_POINT('Origin',(0.,0.,0.));
#10447=CARTESIAN_POINT('',(-1.03941116641111,0.,-0.690454891028199));
#10448=CARTESIAN_POINT('Origin',(-0.993747566553533,0.,-0.721999869202979));
#10449=CARTESIAN_POINT('',(-0.977857337884347,0.,-0.775176467748213));
#10450=CARTESIAN_POINT('Origin',(0.,0.,0.));
#10451=CARTESIAN_POINT('',(-0.918603348636235,0.,-0.844553975349802));
#10452=CARTESIAN_POINT('Origin',(-0.86856722168183,0.,-0.86856722168183));
#10453=CARTESIAN_POINT('',(-0.844553975349802,0.,-0.918603348636235));
#10454=CARTESIAN_POINT('Origin',(0.,0.,0.));
#10455=CARTESIAN_POINT('',(-0.775176467748213,0.,-0.977857337884347));
#10456=CARTESIAN_POINT('Origin',(-0.721999869202979,0.,-0.993747566553533));
#10457=CARTESIAN_POINT('',(-0.690454891028198,0.,-1.03941116641111));
#10458=CARTESIAN_POINT('Origin',(0.,0.,0.));
#10459=CARTESIAN_POINT('',(-0.612662169561031,0.,-1.08708260743774));
#10460=CARTESIAN_POINT('Origin',(-0.557654483764164,0.,-1.0944585482776));
#10461=CARTESIAN_POINT('',(-0.519354515801074,0.,-1.13462523166105));
#10462=CARTESIAN_POINT('Origin',(0.,0.,0.));
#10463=CARTESIAN_POINT('',(-0.43506209545009,0.,-1.16954029537568));
#10464=CARTESIAN_POINT('Origin',(-0.379577794185951,0.,-1.1682203282434));
#10465=CARTESIAN_POINT('',(-0.33546590875611,0.,-1.20190105810224));
#10466=CARTESIAN_POINT('Origin',(0.,0.,0.));
#10467=CARTESIAN_POINT('',(-0.246749348660854,0.,-1.22320001975977));
#10468=CARTESIAN_POINT('Origin',(-0.192154639568406,0.,-1.21321664662686));
#10469=CARTESIAN_POINT('',(-0.14331701769005,0.,-1.23958209161204));
#10470=CARTESIAN_POINT('Origin',(0.,0.,0.));
#10471=CARTESIAN_POINT('',(-0.052360813993451,0.,-1.24674050008925));
#10472=CARTESIAN_POINT('Origin',(7.52141045863017E-17,0.,-1.22833954473516));
#10473=CARTESIAN_POINT('',(0.0523608139934511,0.,-1.24674050008925));
#10474=CARTESIAN_POINT('Origin',(0.,0.,0.));
#10475=CARTESIAN_POINT('',(0.14331701769005,0.,-1.23958209161204));
#10476=CARTESIAN_POINT('Origin',(0.192154639568406,0.,-1.21321664662686));
#10477=CARTESIAN_POINT('',(0.246749348660855,0.,-1.22320001975977));
#10478=CARTESIAN_POINT('Origin',(0.,0.,0.));
#10479=CARTESIAN_POINT('',(0.33546590875611,0.,-1.20190105810224));
#10480=CARTESIAN_POINT('Origin',(0.379577794185951,0.,-1.1682203282434));
#10481=CARTESIAN_POINT('',(0.43506209545009,0.,-1.16954029537568));
#10482=CARTESIAN_POINT('Origin',(0.,0.,0.));
#10483=CARTESIAN_POINT('',(0.519354515801074,0.,-1.13462523166105));
#10484=CARTESIAN_POINT('Origin',(0.557654483764164,0.,-1.0944585482776));
#10485=CARTESIAN_POINT('',(0.612662169561031,0.,-1.08708260743774));
#10486=CARTESIAN_POINT('Origin',(0.,0.,0.));
#10487=CARTESIAN_POINT('',(0.690454891028198,0.,-1.03941116641111));
#10488=CARTESIAN_POINT('Origin',(0.721999869202979,0.,-0.993747566553533));
#10489=CARTESIAN_POINT('',(0.775176467748213,0.,-0.977857337884347));
#10490=CARTESIAN_POINT('Origin',(0.,0.,0.));
#10491=CARTESIAN_POINT('',(0.844553975349802,0.,-0.918603348636235));
#10492=CARTESIAN_POINT('Origin',(0.86856722168183,0.,-0.86856722168183));
#10493=CARTESIAN_POINT('',(0.918603348636235,0.,-0.844553975349802));
#10494=CARTESIAN_POINT('Origin',(0.,0.,0.));
#10495=CARTESIAN_POINT('',(0.977857337884347,0.,-0.775176467748213));
#10496=CARTESIAN_POINT('Origin',(0.993747566553533,0.,-0.721999869202979));
#10497=CARTESIAN_POINT('',(1.03941116641111,0.,-0.690454891028198));
#10498=CARTESIAN_POINT('Origin',(0.,0.,0.));
#10499=CARTESIAN_POINT('',(1.08708260743774,0.,-0.612662169561031));
#10500=CARTESIAN_POINT('Origin',(1.0944585482776,0.,-0.557654483764164));
#10501=CARTESIAN_POINT('',(1.13462523166105,0.,-0.519354515801074));
#10502=CARTESIAN_POINT('Origin',(0.,0.,0.));
#10503=CARTESIAN_POINT('',(1.16954029537568,0.,-0.43506209545009));
#10504=CARTESIAN_POINT('Origin',(1.1682203282434,0.,-0.379577794185951));
#10505=CARTESIAN_POINT('',(1.20190105810224,0.,-0.33546590875611));
#10506=CARTESIAN_POINT('Origin',(0.,0.,0.));
#10507=CARTESIAN_POINT('',(1.22320001975977,0.,-0.246749348660855));
#10508=CARTESIAN_POINT('Origin',(1.21321664662686,0.,-0.192154639568406));
#10509=CARTESIAN_POINT('',(1.23958209161204,0.,-0.14331701769005));
#10510=CARTESIAN_POINT('Origin',(0.,0.,0.));
#10511=CARTESIAN_POINT('',(1.24674050008925,0.,0.052360813993451));
#10512=CARTESIAN_POINT('Origin',(1.22833954473516,0.,0.));
#10513=CARTESIAN_POINT('',(1.24674050008925,0.,-0.052360813993451));
#10514=CARTESIAN_POINT('Origin',(0.,0.,0.));
#10515=CARTESIAN_POINT('',(0.,0.,0.));
#10516=CARTESIAN_POINT('Origin',(0.7,0.,0.25));
#10517=CARTESIAN_POINT('',(0.7,0.16,0.4));
#10518=CARTESIAN_POINT('',(0.7,0.2,0.36));
#10519=CARTESIAN_POINT('',(0.7,0.1675,0.3925));
#10520=CARTESIAN_POINT('',(0.7,-0.16,0.4));
#10521=CARTESIAN_POINT('',(0.7,0.,0.4));
#10522=CARTESIAN_POINT('',(0.7,-0.2,0.36));
#10523=CARTESIAN_POINT('',(0.7,-0.1675,0.3925));
#10524=CARTESIAN_POINT('',(0.7,-0.2,0.04));
#10525=CARTESIAN_POINT('',(0.7,-0.2,0.125));
#10526=CARTESIAN_POINT('',(0.7,-0.16,0.));
#10527=CARTESIAN_POINT('',(0.7,-0.1925,0.0325));
#10528=CARTESIAN_POINT('',(0.7,0.16,0.));
#10529=CARTESIAN_POINT('',(0.7,0.,0.));
#10530=CARTESIAN_POINT('',(0.7,0.2,0.04));
#10531=CARTESIAN_POINT('',(0.7,0.1925,0.0325));
#10532=CARTESIAN_POINT('',(0.7,0.2,0.125));
#10533=CARTESIAN_POINT('Origin',(-0.4,-0.18,0.02));
#10534=CARTESIAN_POINT('',(-0.7,-0.2,0.04));
#10535=CARTESIAN_POINT('',(-0.4,-0.2,0.04));
#10536=CARTESIAN_POINT('',(-0.7,-0.16,0.));
#10537=CARTESIAN_POINT('',(-0.7,-0.1925,0.0325));
#10538=CARTESIAN_POINT('',(-0.4,-0.16,0.));
#10539=CARTESIAN_POINT('Origin',(-0.8,-0.2,0.));
#10540=CARTESIAN_POINT('',(-0.7,-0.2,0.36));
#10541=CARTESIAN_POINT('',(-0.4,-0.2,0.36));
#10542=CARTESIAN_POINT('',(-0.7,-0.2,0.125));
#10543=CARTESIAN_POINT('Origin',(-0.4,-0.18,0.38));
#10544=CARTESIAN_POINT('',(-0.7,-0.16,0.4));
#10545=CARTESIAN_POINT('',(-0.4,-0.16,0.4));
#10546=CARTESIAN_POINT('',(-0.7,-0.1675,0.3925));
#10547=CARTESIAN_POINT('Origin',(0.,0.,0.4));
#10548=CARTESIAN_POINT('',(-0.7,0.16,0.4));
#10549=CARTESIAN_POINT('',(0.4,0.16,0.4));
#10550=CARTESIAN_POINT('',(-0.7,0.,0.4));
#10551=CARTESIAN_POINT('Origin',(-0.7,0.,0.25));
#10552=CARTESIAN_POINT('',(-0.7,0.2,0.36));
#10553=CARTESIAN_POINT('',(-0.7,0.1675,0.3925));
#10554=CARTESIAN_POINT('',(-0.7,0.2,0.04));
#10555=CARTESIAN_POINT('',(-0.7,0.2,0.125));
#10556=CARTESIAN_POINT('',(-0.7,0.16,0.));
#10557=CARTESIAN_POINT('',(-0.7,0.1925,0.0325));
#10558=CARTESIAN_POINT('',(-0.7,0.,0.));
#10559=CARTESIAN_POINT('Origin',(0.4,0.18,0.38));
#10560=CARTESIAN_POINT('',(0.4,0.2,0.36));
#10561=CARTESIAN_POINT('Origin',(0.8,0.2,0.));
#10562=CARTESIAN_POINT('',(0.4,0.2,0.04));
#10563=CARTESIAN_POINT('Origin',(0.4,0.18,0.02));
#10564=CARTESIAN_POINT('',(0.4,0.16,0.));
#10565=CARTESIAN_POINT('Origin',(0.,0.,0.));
#10566=CARTESIAN_POINT('',(0.,0.,0.));
#10567=CARTESIAN_POINT('Origin',(0.375,0.5,0.));
#10568=CARTESIAN_POINT('',(-0.375,0.5,-4.59242549680257E-17));
#10569=CARTESIAN_POINT('Origin',(0.,0.5,0.));
#10570=CARTESIAN_POINT('Origin',(0.,0.475,0.));
#10571=CARTESIAN_POINT('',(-0.425,0.45,-5.20474889637625E-17));
#10572=CARTESIAN_POINT('Origin',(0.,0.45,0.));
#10573=CARTESIAN_POINT('',(-0.4,0.475,-4.89858719658941E-17));
#10574=CARTESIAN_POINT('Origin',(0.,0.24,0.));
#10575=CARTESIAN_POINT('',(-0.425,0.0299999999999998,-5.20474889637625E-17));
#10576=CARTESIAN_POINT('Origin',(0.,0.0299999999999998,0.));
#10577=CARTESIAN_POINT('',(-0.425,0.24,-5.20474889637625E-17));
#10578=CARTESIAN_POINT('Origin',(0.,0.0150000000000001,0.));
#10579=CARTESIAN_POINT('',(-0.395,4.85722573273506E-17,-4.83735485663204E-17));
#10580=CARTESIAN_POINT('Origin',(0.,0.,0.));
#10581=CARTESIAN_POINT('',(-0.41,0.0150000000000001,-5.02105187650415E-17));
#10582=CARTESIAN_POINT('Origin',(0.27,0.,0.));
#10583=CARTESIAN_POINT('',(-0.27,0.,-3.30654635769785E-17));
#10584=CARTESIAN_POINT('Origin',(0.,0.,0.));
#10585=CARTESIAN_POINT('Origin',(0.,-0.02,0.));
#10586=CARTESIAN_POINT('',(-0.24505,-0.0498999999999999,3.00099698131059E-17));
#10587=CARTESIAN_POINT('Origin',(0.,-0.0498999999999999,0.));
#10588=CARTESIAN_POINT('',(-0.26,-0.02,-3.18408167778312E-17));
#10589=CARTESIAN_POINT('Origin',(0.,-0.995,0.));
#10590=CARTESIAN_POINT('',(-0.24505,-1.95495,3.00099698131059E-17));
#10591=CARTESIAN_POINT('Origin',(0.,-1.95495,0.));
#10592=CARTESIAN_POINT('',(-0.24505,-0.995,-3.00099698131059E-17));
#10593=CARTESIAN_POINT('Origin',(0.,-1.975,0.));
#10594=CARTESIAN_POINT('',(-0.2,-2.,-2.44929359829471E-17));
#10595=CARTESIAN_POINT('Origin',(0.,-2.,0.));
#10596=CARTESIAN_POINT('',(-0.225,-1.975,-2.75545529808154E-17));
#10597=CARTESIAN_POINT('Origin',(0.,-2.,0.));
#10598=CARTESIAN_POINT('Origin',(0.115470053837925,-0.5,-0.2));
#10599=CARTESIAN_POINT('',(0.23094010767585,-0.5,0.));
#10600=CARTESIAN_POINT('',(0.115470053837925,-0.5,-0.2));
#10601=CARTESIAN_POINT('',(0.23094010767585,-0.5,0.));
#10602=CARTESIAN_POINT('',(0.115470053837925,-0.8,-0.2));
#10603=CARTESIAN_POINT('',(0.115470053837925,-0.5,-0.2));
#10604=CARTESIAN_POINT('',(0.23094010767585,-0.8,0.));
#10605=CARTESIAN_POINT('',(0.23094010767585,-0.8,0.));
#10606=CARTESIAN_POINT('',(0.23094010767585,-0.5,0.));
#10607=CARTESIAN_POINT('Origin',(-0.115470053837925,-0.5,-0.2));
#10608=CARTESIAN_POINT('',(-0.115470053837925,-0.5,-0.2));
#10609=CARTESIAN_POINT('',(0.115470053837925,-0.5,-0.2));
#10610=CARTESIAN_POINT('',(-0.115470053837925,-0.8,-0.2));
#10611=CARTESIAN_POINT('',(-0.115470053837925,-0.5,-0.2));
#10612=CARTESIAN_POINT('',(0.115470053837925,-0.8,-0.2));
#10613=CARTESIAN_POINT('Origin',(-0.23094010767585,-0.5,-2.77555756156289E-17));
#10614=CARTESIAN_POINT('',(-0.23094010767585,-0.5,-2.82820063659975E-17));
#10615=CARTESIAN_POINT('',(-0.115470053837925,-0.5,-0.2));
#10616=CARTESIAN_POINT('',(-0.23094010767585,-0.8,-2.77555756156289E-17));
#10617=CARTESIAN_POINT('',(-0.23094010767585,-0.5,-2.82820063659975E-17));
#10618=CARTESIAN_POINT('',(-0.115470053837925,-0.8,-0.2));
#10619=CARTESIAN_POINT('Origin',(-0.115470053837925,-0.5,0.2));
#10620=CARTESIAN_POINT('',(-0.115470053837925,-0.5,0.2));
#10621=CARTESIAN_POINT('',(-0.23094010767585,-0.5,-2.82820063659975E-17));
#10622=CARTESIAN_POINT('',(-0.115470053837925,-0.8,0.2));
#10623=CARTESIAN_POINT('',(-0.115470053837925,-0.5,0.2));
#10624=CARTESIAN_POINT('',(-0.23094010767585,-0.8,-2.82820063659975E-17));
#10625=CARTESIAN_POINT('Origin',(0.115470053837925,-0.5,0.2));
#10626=CARTESIAN_POINT('',(0.115470053837925,-0.5,0.2));
#10627=CARTESIAN_POINT('',(-0.115470053837925,-0.5,0.2));
#10628=CARTESIAN_POINT('',(0.115470053837925,-0.8,0.2));
#10629=CARTESIAN_POINT('',(0.115470053837925,-0.5,0.2));
#10630=CARTESIAN_POINT('',(-0.115470053837925,-0.8,0.2));
#10631=CARTESIAN_POINT('Origin',(0.23094010767585,-0.5,0.));
#10632=CARTESIAN_POINT('',(0.115470053837925,-0.5,0.2));
#10633=CARTESIAN_POINT('',(0.115470053837925,-0.8,0.2));
#10634=CARTESIAN_POINT('Origin',(0.,-0.5,0.));
#10635=CARTESIAN_POINT('Origin',(0.,-0.8,0.));
#10636=CARTESIAN_POINT('',(0.,0.,0.));
#10637=CARTESIAN_POINT('Origin',(-1.,0.,0.35));
#10638=CARTESIAN_POINT('',(-1.,-0.26,0.6));
#10639=CARTESIAN_POINT('',(-1.,-0.3,0.56));
#10640=CARTESIAN_POINT('',(-1.,-0.2675,0.5925));
#10641=CARTESIAN_POINT('',(-1.,0.26,0.6));
#10642=CARTESIAN_POINT('',(-1.,0.,0.6));
#10643=CARTESIAN_POINT('',(-1.,0.3,0.56));
#10644=CARTESIAN_POINT('',(-1.,0.2675,0.5925));
#10645=CARTESIAN_POINT('',(-1.,0.3,0.04));
#10646=CARTESIAN_POINT('',(-1.,0.3,0.175));
#10647=CARTESIAN_POINT('',(-1.,0.26,0.));
#10648=CARTESIAN_POINT('',(-1.,0.2925,0.0325));
#10649=CARTESIAN_POINT('',(-1.,-0.26,0.));
#10650=CARTESIAN_POINT('',(-1.,0.,0.));
#10651=CARTESIAN_POINT('',(-1.,-0.3,0.04));
#10652=CARTESIAN_POINT('',(-1.,-0.2925,0.0325));
#10653=CARTESIAN_POINT('',(-1.,-0.3,0.175));
#10654=CARTESIAN_POINT('Origin',(0.75,0.28,0.02));
#10655=CARTESIAN_POINT('',(1.,0.3,0.04));
#10656=CARTESIAN_POINT('',(0.75,0.3,0.04));
#10657=CARTESIAN_POINT('',(1.,0.26,0.));
#10658=CARTESIAN_POINT('',(1.,0.2925,0.0325));
#10659=CARTESIAN_POINT('',(0.75,0.26,0.));
#10660=CARTESIAN_POINT('Origin',(1.5,0.3,0.));
#10661=CARTESIAN_POINT('',(1.,0.3,0.56));
#10662=CARTESIAN_POINT('',(0.75,0.3,0.56));
#10663=CARTESIAN_POINT('',(1.,0.3,0.175));
#10664=CARTESIAN_POINT('Origin',(0.75,0.28,0.58));
#10665=CARTESIAN_POINT('',(1.,0.26,0.6));
#10666=CARTESIAN_POINT('',(0.75,0.26,0.6));
#10667=CARTESIAN_POINT('',(1.,0.2675,0.5925));
#10668=CARTESIAN_POINT('Origin',(0.,0.,0.6));
#10669=CARTESIAN_POINT('',(1.,-0.26,0.6));
#10670=CARTESIAN_POINT('',(-0.75,-0.26,0.6));
#10671=CARTESIAN_POINT('',(1.,0.,0.6));
#10672=CARTESIAN_POINT('Origin',(1.,0.,0.35));
#10673=CARTESIAN_POINT('',(1.,-0.26,0.));
#10674=CARTESIAN_POINT('',(1.,-0.3,0.04));
#10675=CARTESIAN_POINT('',(1.,-0.2925,0.0325));
#10676=CARTESIAN_POINT('',(1.,0.,0.));
#10677=CARTESIAN_POINT('',(1.,-0.3,0.56));
#10678=CARTESIAN_POINT('',(1.,-0.2675,0.5925));
#10679=CARTESIAN_POINT('',(1.,-0.3,0.175));
#10680=CARTESIAN_POINT('Origin',(0.,0.,0.));
#10681=CARTESIAN_POINT('',(-0.75,-0.26,0.));
#10682=CARTESIAN_POINT('Origin',(-0.75,-0.28,0.58));
#10683=CARTESIAN_POINT('',(-0.75,-0.3,0.56));
#10684=CARTESIAN_POINT('Origin',(-0.75,-0.28,0.02));
#10685=CARTESIAN_POINT('',(-0.75,-0.3,0.04));
#10686=CARTESIAN_POINT('Origin',(-1.5,-0.3,0.));
#10687=CARTESIAN_POINT('',(0.,0.,0.));
#10688=CARTESIAN_POINT('Origin',(0.0721687836487032,0.,-0.125));
#10689=CARTESIAN_POINT('',(0.0721687836487032,0.,-0.125));
#10690=CARTESIAN_POINT('',(0.144337567297406,0.,0.));
#10691=CARTESIAN_POINT('',(0.117710979560879,0.,-0.0461186027918559));
#10692=CARTESIAN_POINT('',(0.0721687836487032,-0.25,-0.125));
#10693=CARTESIAN_POINT('',(0.0721687836487032,0.,-0.125));
#10694=CARTESIAN_POINT('',(0.144337567297406,-0.25,0.));
#10695=CARTESIAN_POINT('',(0.144337567297406,-0.25,0.));
#10696=CARTESIAN_POINT('',(0.144337567297406,0.,0.));
#10697=CARTESIAN_POINT('Origin',(-0.0721687836487032,0.,-0.125));
#10698=CARTESIAN_POINT('',(-0.0721687836487032,0.,-0.125));
#10699=CARTESIAN_POINT('',(0.0739156081756484,0.,-0.125));
#10700=CARTESIAN_POINT('',(-0.0721687836487032,-0.25,-0.125));
#10701=CARTESIAN_POINT('',(-0.0721687836487032,0.,-0.125));
#10702=CARTESIAN_POINT('',(0.0721687836487032,-0.25,-0.125));
#10703=CARTESIAN_POINT('Origin',(-0.144337567297406,0.,-4.16333634234434E-17));
#10704=CARTESIAN_POINT('',(-0.144337567297406,0.,-1.76762539787485E-17));
#10705=CARTESIAN_POINT('',(-0.0987953713852306,0.,-0.0788813972081442));
#10706=CARTESIAN_POINT('',(-0.144337567297406,-0.25,-2.77555756156289E-17));
#10707=CARTESIAN_POINT('',(-0.144337567297406,0.,-1.76762539787485E-17));
#10708=CARTESIAN_POINT('',(-0.0721687836487032,-0.25,-0.125));
#10709=CARTESIAN_POINT('Origin',(-0.0721687836487033,0.,0.125));
#10710=CARTESIAN_POINT('',(-0.0721687836487033,0.,0.125));
#10711=CARTESIAN_POINT('',(-0.0627109795608791,0.,0.141381397208144));
#10712=CARTESIAN_POINT('',(-0.0721687836487033,-0.25,0.125));
#10713=CARTESIAN_POINT('',(-0.0721687836487033,0.,0.125));
#10714=CARTESIAN_POINT('',(-0.144337567297406,-0.25,-1.76762539787485E-17));
#10715=CARTESIAN_POINT('Origin',(0.0721687836487032,0.,0.125));
#10716=CARTESIAN_POINT('',(0.0721687836487032,0.,0.125));
#10717=CARTESIAN_POINT('',(0.146084391824352,0.,0.125));
#10718=CARTESIAN_POINT('',(0.0721687836487032,-0.25,0.125));
#10719=CARTESIAN_POINT('',(0.0721687836487032,0.,0.125));
#10720=CARTESIAN_POINT('',(-0.0721687836487033,-0.25,0.125));
#10721=CARTESIAN_POINT('Origin',(0.144337567297406,0.,0.));
#10722=CARTESIAN_POINT('',(0.153795371385231,0.,-0.0163813972081441));
#10723=CARTESIAN_POINT('',(0.0721687836487032,-0.25,0.125));
#10724=CARTESIAN_POINT('Origin',(0.,-0.25,0.));
#10725=CARTESIAN_POINT('Origin',(0.22,0.,0.));
#10726=CARTESIAN_POINT('',(-0.22,-8.67361737988404E-18,-2.69422295812418E-17));
#10727=CARTESIAN_POINT('Origin',(0.,0.,0.));
#10728=CARTESIAN_POINT('Origin',(0.,-0.015,0.));
#10729=CARTESIAN_POINT('',(-0.24505,-0.02505,-3.00099698131059E-17));
#10730=CARTESIAN_POINT('Origin',(0.,-0.02505,0.));
#10731=CARTESIAN_POINT('',(-0.235,-0.015,-2.87791997799628E-17));
#10732=CARTESIAN_POINT('Origin',(0.,-0.3775,0.));
#10733=CARTESIAN_POINT('',(-0.24505,-0.72995,3.00099698131059E-17));
#10734=CARTESIAN_POINT('Origin',(0.,-0.72995,0.));
#10735=CARTESIAN_POINT('',(-0.24505,-0.3775,-3.00099698131059E-17));
#10736=CARTESIAN_POINT('Origin',(0.,-0.7625,0.));
#10737=CARTESIAN_POINT('',(-0.175,-0.8,-2.14313189850787E-17));
#10738=CARTESIAN_POINT('Origin',(0.,-0.8,0.));
#10739=CARTESIAN_POINT('',(-0.2125,-0.7625,-2.60237444818813E-17));
#10740=CARTESIAN_POINT('Origin',(0.,-0.8,0.));
#10741=CARTESIAN_POINT('',(0.,0.,0.));
#10742=CARTESIAN_POINT('',(0.,0.,0.));
#10743=CARTESIAN_POINT('',(0.,0.,0.));
#10744=CARTESIAN_POINT('',(0.,0.,0.));
#10745=CARTESIAN_POINT('',(0.,0.,0.));
#10746=CARTESIAN_POINT('',(0.,0.,0.));
#10747=CARTESIAN_POINT('',(0.,0.,0.));
#10748=CARTESIAN_POINT('',(0.,0.,0.));
#10749=CARTESIAN_POINT('',(0.,0.,0.));
#10750=CARTESIAN_POINT('',(0.,-4.3,4.53));
#10751=CARTESIAN_POINT('',(0.,-4.325,4.18));
#10752=CARTESIAN_POINT('',(0.,24.9,4.53));
#10753=CARTESIAN_POINT('',(6.35036208909613E-31,24.875,4.18));
#10754=CARTESIAN_POINT('',(0.,-5.7,4.53));
#10755=CARTESIAN_POINT('',(0.,27.2,4.53));
#10756=CARTESIAN_POINT('',(0.,10.2,3.88));
#10757=CARTESIAN_POINT('',(0.,10.2,6.33));
#10758=CARTESIAN_POINT('',(0.,-1.25,6.33));
#10759=CARTESIAN_POINT('',(0.,22.85,6.33));
#10760=CARTESIAN_POINT('',(0.,0.,0.));
#10761=CARTESIAN_POINT('',(0.,0.,0.));
#10762=UNCERTAINTY_MEASURE_WITH_UNIT(LENGTH_MEASURE(0.001),#10822,
'DISTANCE_ACCURACY_VALUE',
'Maximum model space distance between geometric entities at asserted c
onnectivities');
#10763=UNCERTAINTY_MEASURE_WITH_UNIT(LENGTH_MEASURE(0.001),#10822,
'DISTANCE_ACCURACY_VALUE',
'Maximum model space distance between geometric entities at asserted c
onnectivities');
#10764=UNCERTAINTY_MEASURE_WITH_UNIT(LENGTH_MEASURE(0.001),#10822,
'DISTANCE_ACCURACY_VALUE',
'Maximum model space distance between geometric entities at asserted c
onnectivities');
#10765=UNCERTAINTY_MEASURE_WITH_UNIT(LENGTH_MEASURE(0.001),#10822,
'DISTANCE_ACCURACY_VALUE',
'Maximum model space distance between geometric entities at asserted c
onnectivities');
#10766=UNCERTAINTY_MEASURE_WITH_UNIT(LENGTH_MEASURE(0.001),#10822,
'DISTANCE_ACCURACY_VALUE',
'Maximum model space distance between geometric entities at asserted c
onnectivities');
#10767=UNCERTAINTY_MEASURE_WITH_UNIT(LENGTH_MEASURE(0.001),#10822,
'DISTANCE_ACCURACY_VALUE',
'Maximum model space distance between geometric entities at asserted c
onnectivities');
#10768=UNCERTAINTY_MEASURE_WITH_UNIT(LENGTH_MEASURE(0.001),#10822,
'DISTANCE_ACCURACY_VALUE',
'Maximum model space distance between geometric entities at asserted c
onnectivities');
#10769=UNCERTAINTY_MEASURE_WITH_UNIT(LENGTH_MEASURE(0.001),#10822,
'DISTANCE_ACCURACY_VALUE',
'Maximum model space distance between geometric entities at asserted c
onnectivities');
#10770=UNCERTAINTY_MEASURE_WITH_UNIT(LENGTH_MEASURE(0.001),#10822,
'DISTANCE_ACCURACY_VALUE',
'Maximum model space distance between geometric entities at asserted c
onnectivities');
#10771=UNCERTAINTY_MEASURE_WITH_UNIT(LENGTH_MEASURE(0.001),#10822,
'DISTANCE_ACCURACY_VALUE',
'Maximum model space distance between geometric entities at asserted c
onnectivities');
#10772=UNCERTAINTY_MEASURE_WITH_UNIT(LENGTH_MEASURE(0.001),#10822,
'DISTANCE_ACCURACY_VALUE',
'Maximum model space distance between geometric entities at asserted c
onnectivities');
#10773=UNCERTAINTY_MEASURE_WITH_UNIT(LENGTH_MEASURE(0.001),#10822,
'DISTANCE_ACCURACY_VALUE',
'Maximum model space distance between geometric entities at asserted c
onnectivities');
#10774=UNCERTAINTY_MEASURE_WITH_UNIT(LENGTH_MEASURE(0.001),#10822,
'DISTANCE_ACCURACY_VALUE',
'Maximum model space distance between geometric entities at asserted c
onnectivities');
#10775=UNCERTAINTY_MEASURE_WITH_UNIT(LENGTH_MEASURE(0.001),#10822,
'DISTANCE_ACCURACY_VALUE',
'Maximum model space distance between geometric entities at asserted c
onnectivities');
#10776=UNCERTAINTY_MEASURE_WITH_UNIT(LENGTH_MEASURE(0.001),#10822,
'DISTANCE_ACCURACY_VALUE',
'Maximum model space distance between geometric entities at asserted c
onnectivities');
#10777=UNCERTAINTY_MEASURE_WITH_UNIT(LENGTH_MEASURE(0.001),#10822,
'DISTANCE_ACCURACY_VALUE',
'Maximum model space distance between geometric entities at asserted c
onnectivities');
#10778=UNCERTAINTY_MEASURE_WITH_UNIT(LENGTH_MEASURE(0.001),#10822,
'DISTANCE_ACCURACY_VALUE',
'Maximum model space distance between geometric entities at asserted c
onnectivities');
#10779=UNCERTAINTY_MEASURE_WITH_UNIT(LENGTH_MEASURE(0.001),#10822,
'DISTANCE_ACCURACY_VALUE',
'Maximum model space distance between geometric entities at asserted c
onnectivities');
#10780=UNCERTAINTY_MEASURE_WITH_UNIT(LENGTH_MEASURE(0.001),#10822,
'DISTANCE_ACCURACY_VALUE',
'Maximum model space distance between geometric entities at asserted c
onnectivities');
#10781=UNCERTAINTY_MEASURE_WITH_UNIT(LENGTH_MEASURE(0.001),#10822,
'DISTANCE_ACCURACY_VALUE',
'Maximum model space distance between geometric entities at asserted c
onnectivities');
#10782=UNCERTAINTY_MEASURE_WITH_UNIT(LENGTH_MEASURE(0.001),#10822,
'DISTANCE_ACCURACY_VALUE',
'Maximum model space distance between geometric entities at asserted c
onnectivities');
#10783=UNCERTAINTY_MEASURE_WITH_UNIT(LENGTH_MEASURE(0.001),#10822,
'DISTANCE_ACCURACY_VALUE',
'Maximum model space distance between geometric entities at asserted c
onnectivities');
#10784=UNCERTAINTY_MEASURE_WITH_UNIT(LENGTH_MEASURE(0.001),#10822,
'DISTANCE_ACCURACY_VALUE',
'Maximum model space distance between geometric entities at asserted c
onnectivities');
#10785=UNCERTAINTY_MEASURE_WITH_UNIT(LENGTH_MEASURE(0.001),#10822,
'DISTANCE_ACCURACY_VALUE',
'Maximum model space distance between geometric entities at asserted c
onnectivities');
#10786=UNCERTAINTY_MEASURE_WITH_UNIT(LENGTH_MEASURE(0.001),#10822,
'DISTANCE_ACCURACY_VALUE',
'Maximum model space distance between geometric entities at asserted c
onnectivities');
#10787=UNCERTAINTY_MEASURE_WITH_UNIT(LENGTH_MEASURE(0.001),#10822,
'DISTANCE_ACCURACY_VALUE',
'Maximum model space distance between geometric entities at asserted c
onnectivities');
#10788=UNCERTAINTY_MEASURE_WITH_UNIT(LENGTH_MEASURE(0.001),#10822,
'DISTANCE_ACCURACY_VALUE',
'Maximum model space distance between geometric entities at asserted c
onnectivities');
#10789=UNCERTAINTY_MEASURE_WITH_UNIT(LENGTH_MEASURE(0.001),#10822,
'DISTANCE_ACCURACY_VALUE',
'Maximum model space distance between geometric entities at asserted c
onnectivities');
#10790=UNCERTAINTY_MEASURE_WITH_UNIT(LENGTH_MEASURE(0.001),#10822,
'DISTANCE_ACCURACY_VALUE',
'Maximum model space distance between geometric entities at asserted c
onnectivities');
#10791=UNCERTAINTY_MEASURE_WITH_UNIT(LENGTH_MEASURE(0.001),#10822,
'DISTANCE_ACCURACY_VALUE',
'Maximum model space distance between geometric entities at asserted c
onnectivities');
#10792=(
GEOMETRIC_REPRESENTATION_CONTEXT(3)
GLOBAL_UNCERTAINTY_ASSIGNED_CONTEXT((#10762))
GLOBAL_UNIT_ASSIGNED_CONTEXT((#10822,#10824,#10825))
REPRESENTATION_CONTEXT('','3D')
);
#10793=(
GEOMETRIC_REPRESENTATION_CONTEXT(3)
GLOBAL_UNCERTAINTY_ASSIGNED_CONTEXT((#10763))
GLOBAL_UNIT_ASSIGNED_CONTEXT((#10822,#10824,#10825))
REPRESENTATION_CONTEXT('','3D')
);
#10794=(
GEOMETRIC_REPRESENTATION_CONTEXT(3)
GLOBAL_UNCERTAINTY_ASSIGNED_CONTEXT((#10764))
GLOBAL_UNIT_ASSIGNED_CONTEXT((#10822,#10824,#10825))
REPRESENTATION_CONTEXT('','3D')
);
#10795=(
GEOMETRIC_REPRESENTATION_CONTEXT(3)
GLOBAL_UNCERTAINTY_ASSIGNED_CONTEXT((#10765))
GLOBAL_UNIT_ASSIGNED_CONTEXT((#10822,#10824,#10825))
REPRESENTATION_CONTEXT('','3D')
);
#10796=(
GEOMETRIC_REPRESENTATION_CONTEXT(3)
GLOBAL_UNCERTAINTY_ASSIGNED_CONTEXT((#10766))
GLOBAL_UNIT_ASSIGNED_CONTEXT((#10822,#10824,#10825))
REPRESENTATION_CONTEXT('','3D')
);
#10797=(
GEOMETRIC_REPRESENTATION_CONTEXT(3)
GLOBAL_UNCERTAINTY_ASSIGNED_CONTEXT((#10767))
GLOBAL_UNIT_ASSIGNED_CONTEXT((#10822,#10824,#10825))
REPRESENTATION_CONTEXT('','3D')
);
#10798=(
GEOMETRIC_REPRESENTATION_CONTEXT(3)
GLOBAL_UNCERTAINTY_ASSIGNED_CONTEXT((#10768))
GLOBAL_UNIT_ASSIGNED_CONTEXT((#10822,#10824,#10825))
REPRESENTATION_CONTEXT('','3D')
);
#10799=(
GEOMETRIC_REPRESENTATION_CONTEXT(3)
GLOBAL_UNCERTAINTY_ASSIGNED_CONTEXT((#10769))
GLOBAL_UNIT_ASSIGNED_CONTEXT((#10822,#10824,#10825))
REPRESENTATION_CONTEXT('','3D')
);
#10800=(
GEOMETRIC_REPRESENTATION_CONTEXT(3)
GLOBAL_UNCERTAINTY_ASSIGNED_CONTEXT((#10770))
GLOBAL_UNIT_ASSIGNED_CONTEXT((#10822,#10824,#10825))
REPRESENTATION_CONTEXT('','3D')
);
#10801=(
GEOMETRIC_REPRESENTATION_CONTEXT(3)
GLOBAL_UNCERTAINTY_ASSIGNED_CONTEXT((#10771))
GLOBAL_UNIT_ASSIGNED_CONTEXT((#10822,#10824,#10825))
REPRESENTATION_CONTEXT('','3D')
);
#10802=(
GEOMETRIC_REPRESENTATION_CONTEXT(3)
GLOBAL_UNCERTAINTY_ASSIGNED_CONTEXT((#10772))
GLOBAL_UNIT_ASSIGNED_CONTEXT((#10822,#10824,#10825))
REPRESENTATION_CONTEXT('','3D')
);
#10803=(
GEOMETRIC_REPRESENTATION_CONTEXT(3)
GLOBAL_UNCERTAINTY_ASSIGNED_CONTEXT((#10773))
GLOBAL_UNIT_ASSIGNED_CONTEXT((#10822,#10824,#10825))
REPRESENTATION_CONTEXT('','3D')
);
#10804=(
GEOMETRIC_REPRESENTATION_CONTEXT(3)
GLOBAL_UNCERTAINTY_ASSIGNED_CONTEXT((#10774))
GLOBAL_UNIT_ASSIGNED_CONTEXT((#10822,#10824,#10825))
REPRESENTATION_CONTEXT('','3D')
);
#10805=(
GEOMETRIC_REPRESENTATION_CONTEXT(3)
GLOBAL_UNCERTAINTY_ASSIGNED_CONTEXT((#10775))
GLOBAL_UNIT_ASSIGNED_CONTEXT((#10822,#10824,#10825))
REPRESENTATION_CONTEXT('','3D')
);
#10806=(
GEOMETRIC_REPRESENTATION_CONTEXT(3)
GLOBAL_UNCERTAINTY_ASSIGNED_CONTEXT((#10776))
GLOBAL_UNIT_ASSIGNED_CONTEXT((#10822,#10824,#10825))
REPRESENTATION_CONTEXT('','3D')
);
#10807=(
GEOMETRIC_REPRESENTATION_CONTEXT(3)
GLOBAL_UNCERTAINTY_ASSIGNED_CONTEXT((#10777))
GLOBAL_UNIT_ASSIGNED_CONTEXT((#10822,#10824,#10825))
REPRESENTATION_CONTEXT('','3D')
);
#10808=(
GEOMETRIC_REPRESENTATION_CONTEXT(3)
GLOBAL_UNCERTAINTY_ASSIGNED_CONTEXT((#10778))
GLOBAL_UNIT_ASSIGNED_CONTEXT((#10822,#10824,#10825))
REPRESENTATION_CONTEXT('','3D')
);
#10809=(
GEOMETRIC_REPRESENTATION_CONTEXT(3)
GLOBAL_UNCERTAINTY_ASSIGNED_CONTEXT((#10779))
GLOBAL_UNIT_ASSIGNED_CONTEXT((#10822,#10824,#10825))
REPRESENTATION_CONTEXT('','3D')
);
#10810=(
GEOMETRIC_REPRESENTATION_CONTEXT(3)
GLOBAL_UNCERTAINTY_ASSIGNED_CONTEXT((#10780))
GLOBAL_UNIT_ASSIGNED_CONTEXT((#10822,#10824,#10825))
REPRESENTATION_CONTEXT('','3D')
);
#10811=(
GEOMETRIC_REPRESENTATION_CONTEXT(3)
GLOBAL_UNCERTAINTY_ASSIGNED_CONTEXT((#10781))
GLOBAL_UNIT_ASSIGNED_CONTEXT((#10822,#10824,#10825))
REPRESENTATION_CONTEXT('','3D')
);
#10812=(
GEOMETRIC_REPRESENTATION_CONTEXT(3)
GLOBAL_UNCERTAINTY_ASSIGNED_CONTEXT((#10782))
GLOBAL_UNIT_ASSIGNED_CONTEXT((#10822,#10824,#10825))
REPRESENTATION_CONTEXT('','3D')
);
#10813=(
GEOMETRIC_REPRESENTATION_CONTEXT(3)
GLOBAL_UNCERTAINTY_ASSIGNED_CONTEXT((#10783))
GLOBAL_UNIT_ASSIGNED_CONTEXT((#10822,#10824,#10825))
REPRESENTATION_CONTEXT('','3D')
);
#10814=(
GEOMETRIC_REPRESENTATION_CONTEXT(3)
GLOBAL_UNCERTAINTY_ASSIGNED_CONTEXT((#10784))
GLOBAL_UNIT_ASSIGNED_CONTEXT((#10822,#10824,#10825))
REPRESENTATION_CONTEXT('','3D')
);
#10815=(
GEOMETRIC_REPRESENTATION_CONTEXT(3)
GLOBAL_UNCERTAINTY_ASSIGNED_CONTEXT((#10785))
GLOBAL_UNIT_ASSIGNED_CONTEXT((#10822,#10824,#10825))
REPRESENTATION_CONTEXT('','3D')
);
#10816=(
GEOMETRIC_REPRESENTATION_CONTEXT(3)
GLOBAL_UNCERTAINTY_ASSIGNED_CONTEXT((#10786))
GLOBAL_UNIT_ASSIGNED_CONTEXT((#10822,#10824,#10825))
REPRESENTATION_CONTEXT('','3D')
);
#10817=(
GEOMETRIC_REPRESENTATION_CONTEXT(3)
GLOBAL_UNCERTAINTY_ASSIGNED_CONTEXT((#10787))
GLOBAL_UNIT_ASSIGNED_CONTEXT((#10822,#10824,#10825))
REPRESENTATION_CONTEXT('','3D')
);
#10818=(
GEOMETRIC_REPRESENTATION_CONTEXT(3)
GLOBAL_UNCERTAINTY_ASSIGNED_CONTEXT((#10788))
GLOBAL_UNIT_ASSIGNED_CONTEXT((#10822,#10824,#10825))
REPRESENTATION_CONTEXT('','3D')
);
#10819=(
GEOMETRIC_REPRESENTATION_CONTEXT(3)
GLOBAL_UNCERTAINTY_ASSIGNED_CONTEXT((#10789))
GLOBAL_UNIT_ASSIGNED_CONTEXT((#10822,#10824,#10825))
REPRESENTATION_CONTEXT('','3D')
);
#10820=(
GEOMETRIC_REPRESENTATION_CONTEXT(3)
GLOBAL_UNCERTAINTY_ASSIGNED_CONTEXT((#10790))
GLOBAL_UNIT_ASSIGNED_CONTEXT((#10822,#10824,#10825))
REPRESENTATION_CONTEXT('','3D')
);
#10821=(
GEOMETRIC_REPRESENTATION_CONTEXT(3)
GLOBAL_UNCERTAINTY_ASSIGNED_CONTEXT((#10791))
GLOBAL_UNIT_ASSIGNED_CONTEXT((#10822,#10824,#10825))
REPRESENTATION_CONTEXT('','3D')
);
#10822=(
LENGTH_UNIT()
NAMED_UNIT(*)
SI_UNIT(.CENTI.,.METRE.)
);
#10823=(
LENGTH_UNIT()
NAMED_UNIT(*)
SI_UNIT($,.METRE.)
);
#10824=(
NAMED_UNIT(*)
PLANE_ANGLE_UNIT()
SI_UNIT($,.RADIAN.)
);
#10825=(
NAMED_UNIT(*)
SI_UNIT($,.STERADIAN.)
SOLID_ANGLE_UNIT()
);
#10826=SHAPE_DEFINITION_REPRESENTATION(#10855,#10924);
#10827=SHAPE_DEFINITION_REPRESENTATION(#10856,#10925);
#10828=SHAPE_DEFINITION_REPRESENTATION(#10857,#10926);
#10829=SHAPE_DEFINITION_REPRESENTATION(#10858,#10927);
#10830=SHAPE_DEFINITION_REPRESENTATION(#10859,#10928);
#10831=SHAPE_DEFINITION_REPRESENTATION(#10860,#10929);
#10832=SHAPE_DEFINITION_REPRESENTATION(#10861,#10930);
#10833=SHAPE_DEFINITION_REPRESENTATION(#10862,#10931);
#10834=SHAPE_DEFINITION_REPRESENTATION(#10863,#10932);
#10835=SHAPE_DEFINITION_REPRESENTATION(#10864,#10933);
#10836=SHAPE_DEFINITION_REPRESENTATION(#10865,#10934);
#10837=SHAPE_DEFINITION_REPRESENTATION(#10866,#10935);
#10838=SHAPE_DEFINITION_REPRESENTATION(#10869,#10936);
#10839=SHAPE_DEFINITION_REPRESENTATION(#10870,#10937);
#10840=SHAPE_DEFINITION_REPRESENTATION(#10888,#10938);
#10841=SHAPE_DEFINITION_REPRESENTATION(#10889,#10939);
#10842=SHAPE_DEFINITION_REPRESENTATION(#10890,#10940);
#10843=SHAPE_DEFINITION_REPRESENTATION(#10891,#10941);
#10844=SHAPE_DEFINITION_REPRESENTATION(#10892,#10942);
#10845=SHAPE_DEFINITION_REPRESENTATION(#10893,#10943);
#10846=SHAPE_DEFINITION_REPRESENTATION(#10894,#10944);
#10847=SHAPE_DEFINITION_REPRESENTATION(#10895,#10945);
#10848=SHAPE_DEFINITION_REPRESENTATION(#10896,#10946);
#10849=SHAPE_DEFINITION_REPRESENTATION(#10897,#10947);
#10850=SHAPE_DEFINITION_REPRESENTATION(#10898,#10948);
#10851=SHAPE_DEFINITION_REPRESENTATION(#10899,#10949);
#10852=SHAPE_DEFINITION_REPRESENTATION(#10900,#10950);
#10853=SHAPE_DEFINITION_REPRESENTATION(#10901,#10951);
#10854=SHAPE_DEFINITION_REPRESENTATION(#10902,#10952);
#10855=PRODUCT_DEFINITION_SHAPE('',$,#10954);
#10856=PRODUCT_DEFINITION_SHAPE('',$,#10955);
#10857=PRODUCT_DEFINITION_SHAPE('',$,#10956);
#10858=PRODUCT_DEFINITION_SHAPE('',$,#10957);
#10859=PRODUCT_DEFINITION_SHAPE('',$,#10958);
#10860=PRODUCT_DEFINITION_SHAPE('',$,#10959);
#10861=PRODUCT_DEFINITION_SHAPE('',$,#10960);
#10862=PRODUCT_DEFINITION_SHAPE('',$,#10961);
#10863=PRODUCT_DEFINITION_SHAPE('',$,#10962);
#10864=PRODUCT_DEFINITION_SHAPE('',$,#10963);
#10865=PRODUCT_DEFINITION_SHAPE('',$,#10964);
#10866=PRODUCT_DEFINITION_SHAPE('',$,#10965);
#10867=PRODUCT_DEFINITION_SHAPE($,$,#144);
#10868=PRODUCT_DEFINITION_SHAPE($,$,#145);
#10869=PRODUCT_DEFINITION_SHAPE('',$,#10966);
#10870=PRODUCT_DEFINITION_SHAPE('',$,#10967);
#10871=PRODUCT_DEFINITION_SHAPE($,$,#146);
#10872=PRODUCT_DEFINITION_SHAPE($,$,#147);
#10873=PRODUCT_DEFINITION_SHAPE($,$,#148);
#10874=PRODUCT_DEFINITION_SHAPE($,$,#149);
#10875=PRODUCT_DEFINITION_SHAPE($,$,#150);
#10876=PRODUCT_DEFINITION_SHAPE($,$,#151);
#10877=PRODUCT_DEFINITION_SHAPE($,$,#152);
#10878=PRODUCT_DEFINITION_SHAPE($,$,#153);
#10879=PRODUCT_DEFINITION_SHAPE($,$,#154);
#10880=PRODUCT_DEFINITION_SHAPE($,$,#155);
#10881=PRODUCT_DEFINITION_SHAPE($,$,#156);
#10882=PRODUCT_DEFINITION_SHAPE($,$,#157);
#10883=PRODUCT_DEFINITION_SHAPE($,$,#158);
#10884=PRODUCT_DEFINITION_SHAPE($,$,#159);
#10885=PRODUCT_DEFINITION_SHAPE($,$,#160);
#10886=PRODUCT_DEFINITION_SHAPE($,$,#161);
#10887=PRODUCT_DEFINITION_SHAPE($,$,#162);
#10888=PRODUCT_DEFINITION_SHAPE('',$,#10968);
#10889=PRODUCT_DEFINITION_SHAPE('',$,#10969);
#10890=PRODUCT_DEFINITION_SHAPE('',$,#10970);
#10891=PRODUCT_DEFINITION_SHAPE('',$,#10971);
#10892=PRODUCT_DEFINITION_SHAPE('',$,#10972);
#10893=PRODUCT_DEFINITION_SHAPE('',$,#10973);
#10894=PRODUCT_DEFINITION_SHAPE('',$,#10974);
#10895=PRODUCT_DEFINITION_SHAPE('',$,#10975);
#10896=PRODUCT_DEFINITION_SHAPE('',$,#10976);
#10897=PRODUCT_DEFINITION_SHAPE('',$,#10977);
#10898=PRODUCT_DEFINITION_SHAPE('',$,#10978);
#10899=PRODUCT_DEFINITION_SHAPE('',$,#10979);
#10900=PRODUCT_DEFINITION_SHAPE('',$,#10980);
#10901=PRODUCT_DEFINITION_SHAPE('',$,#10981);
#10902=PRODUCT_DEFINITION_SHAPE('',$,#10982);
#10903=PRODUCT_DEFINITION_SHAPE($,$,#163);
#10904=PRODUCT_DEFINITION_SHAPE($,$,#164);
#10905=PRODUCT_DEFINITION_SHAPE($,$,#165);
#10906=PRODUCT_DEFINITION_SHAPE($,$,#166);
#10907=PRODUCT_DEFINITION_SHAPE($,$,#167);
#10908=PRODUCT_DEFINITION_SHAPE($,$,#168);
#10909=PRODUCT_DEFINITION_SHAPE($,$,#169);
#10910=PRODUCT_DEFINITION_SHAPE($,$,#170);
#10911=PRODUCT_DEFINITION_SHAPE($,$,#171);
#10912=PRODUCT_DEFINITION_SHAPE($,$,#172);
#10913=PRODUCT_DEFINITION_SHAPE($,$,#173);
#10914=PRODUCT_DEFINITION_SHAPE($,$,#174);
#10915=PRODUCT_DEFINITION_SHAPE($,$,#175);
#10916=PRODUCT_DEFINITION_SHAPE($,$,#176);
#10917=PRODUCT_DEFINITION_SHAPE($,$,#177);
#10918=PRODUCT_DEFINITION_SHAPE($,$,#178);
#10919=PRODUCT_DEFINITION_SHAPE($,$,#179);
#10920=PRODUCT_DEFINITION_SHAPE($,$,#180);
#10921=PRODUCT_DEFINITION_SHAPE($,$,#181);
#10922=PRODUCT_DEFINITION_SHAPE($,$,#182);
#10923=PRODUCT_DEFINITION_SHAPE($,$,#183);
#10924=SHAPE_REPRESENTATION('',(#5877,#6557,#6558),#10792);
#10925=SHAPE_REPRESENTATION('',(#5878,#6053,#6054,#6055,#6056,#6057,#6058,
#6059,#6060,#6061,#6062,#6063,#6064,#6065,#6066,#6067,#6068,#6069),#10793);
#10926=SHAPE_REPRESENTATION('',(#5879),#10794);
#10927=SHAPE_REPRESENTATION('',(#5898),#10795);
#10928=SHAPE_REPRESENTATION('',(#5905),#10796);
#10929=SHAPE_REPRESENTATION('',(#5912),#10797);
#10930=SHAPE_REPRESENTATION('',(#5921),#10798);
#10931=SHAPE_REPRESENTATION('',(#5930),#10799);
#10932=SHAPE_REPRESENTATION('',(#5939),#10800);
#10933=SHAPE_REPRESENTATION('',(#5948,#6018,#6019),#10801);
#10934=SHAPE_REPRESENTATION('',(#5949),#10802);
#10935=SHAPE_REPRESENTATION('',(#5990),#10803);
#10936=SHAPE_REPRESENTATION('',(#6020),#10804);
#10937=SHAPE_REPRESENTATION('',(#6029),#10805);
#10938=SHAPE_REPRESENTATION('',(#6070,#6538,#6539,#6540,#6541,#6542,#6543,
#6544,#6545,#6546,#6547,#6548,#6549,#6550,#6551,#6552,#6553,#6554,#6555,
#6556),#10806);
#10939=SHAPE_REPRESENTATION('',(#6071),#10807);
#10940=SHAPE_REPRESENTATION('',(#6114),#10808);
#10941=SHAPE_REPRESENTATION('',(#6123),#10809);
#10942=SHAPE_REPRESENTATION('',(#6132),#10810);
#10943=SHAPE_REPRESENTATION('',(#6141),#10811);
#10944=SHAPE_REPRESENTATION('',(#6150),#10812);
#10945=SHAPE_REPRESENTATION('',(#6159),#10813);
#10946=SHAPE_REPRESENTATION('',(#6177),#10814);
#10947=SHAPE_REPRESENTATION('',(#6192),#10815);
#10948=SHAPE_REPRESENTATION('',(#6207),#10816);
#10949=SHAPE_REPRESENTATION('',(#6473),#10817);
#10950=SHAPE_REPRESENTATION('',(#6484),#10818);
#10951=SHAPE_REPRESENTATION('',(#6510),#10819);
#10952=SHAPE_REPRESENTATION('',(#6521),#10820);
#10953=PRODUCT_DEFINITION_CONTEXT('part definition',#11042,'design');
#10954=PRODUCT_DEFINITION(
'PAT-025','PAT-025',#10983,#10953);
#10955=PRODUCT_DEFINITION('Pillow block stand','Pillow block stand',#10984,
#10953);
#10956=PRODUCT_DEFINITION('Base channel','Base channel',#10985,#10953);
#10957=PRODUCT_DEFINITION('Bonded pad','Bonded pad',#10986,#10953);
#10958=PRODUCT_DEFINITION('Bonded pad (1)','Bonded pad (1)',#10987,#10953);
#10959=PRODUCT_DEFINITION('Mounting bush','Mounting bush',#10988,#10953);
#10960=PRODUCT_DEFINITION('Mounting bush (1)','Mounting bush (1)',#10989,
#10953);
#10961=PRODUCT_DEFINITION('Mounting bush (2)','Mounting bush (2)',#10990,
#10953);
#10962=PRODUCT_DEFINITION('Mounting bush (3)','Mounting bush (3)',#10991,
#10953);
#10963=PRODUCT_DEFINITION('Pillow Block Bearing - 20 mm Bore',
'Pillow Block Bearing - 20 mm Bore',#10992,#10953);
#10964=PRODUCT_DEFINITION('Housing','Housing',#10993,#10953);
#10965=PRODUCT_DEFINITION('Insert bearing','Insert bearing',#10994,#10953);
#10966=PRODUCT_DEFINITION('Flat Washer - M8','Flat Washer - M8',#10995,
#10953);
#10967=PRODUCT_DEFINITION('M8x25 Bolt','M8x25 Bolt',#10996,#10953);
#10968=PRODUCT_DEFINITION('Countershaft rotor','Countershaft rotor',#10997,
#10953);
#10969=PRODUCT_DEFINITION('Stepped countershaft','Stepped countershaft',
#10998,#10953);
#10970=PRODUCT_DEFINITION('Left spacer','Left spacer',#10999,#10953);
#10971=PRODUCT_DEFINITION('Right spacer','Right spacer',#11000,#10953);
#10972=PRODUCT_DEFINITION('Left end shim','Left end shim',#11001,#10953);
#10973=PRODUCT_DEFINITION('End keeper','End keeper',#11002,#10953);
#10974=PRODUCT_DEFINITION('End keeper (1)','End keeper (1)',#11003,#10953);
#10975=PRODUCT_DEFINITION('Keyed drive hub','Keyed drive hub',#11004,#10953);
#10976=PRODUCT_DEFINITION('Bearing collar','Bearing collar',#11005,#10953);
#10977=PRODUCT_DEFINITION('Bearing collar (1)','Bearing collar (1)',#11006,
#10953);
#10978=PRODUCT_DEFINITION(
'Timing Pulley - 2 mm Pitch, 40 Teeth, 12 mm Bore',
'Timing Pulley - 2 mm Pitch, 40 Teeth, 12 mm Bore',#11007,#10953);
#10979=PRODUCT_DEFINITION('Key 4x4x14','Key 4x4x14',#11008,#10953);
#10980=PRODUCT_DEFINITION('Cap Screw - M5x20','Cap Screw - M5x20',#11009,
#10953);
#10981=PRODUCT_DEFINITION('Key 6x6x20','Key 6x6x20',#11010,#10953);
#10982=PRODUCT_DEFINITION('Socket Set Screw - M5x8',
'Socket Set Screw - M5x8',#11011,#10953);
#10983=PRODUCT_DEFINITION_FORMATION('',$,#11044);
#10984=PRODUCT_DEFINITION_FORMATION('',$,#11045);
#10985=PRODUCT_DEFINITION_FORMATION('',$,#11046);
#10986=PRODUCT_DEFINITION_FORMATION('',$,#11047);
#10987=PRODUCT_DEFINITION_FORMATION('',$,#11048);
#10988=PRODUCT_DEFINITION_FORMATION('',$,#11049);
#10989=PRODUCT_DEFINITION_FORMATION('',$,#11050);
#10990=PRODUCT_DEFINITION_FORMATION('',$,#11051);
#10991=PRODUCT_DEFINITION_FORMATION('',$,#11052);
#10992=PRODUCT_DEFINITION_FORMATION('',$,#11053);
#10993=PRODUCT_DEFINITION_FORMATION('',$,#11054);
#10994=PRODUCT_DEFINITION_FORMATION('',$,#11055);
#10995=PRODUCT_DEFINITION_FORMATION('',$,#11056);
#10996=PRODUCT_DEFINITION_FORMATION('',$,#11057);
#10997=PRODUCT_DEFINITION_FORMATION('',$,#11058);
#10998=PRODUCT_DEFINITION_FORMATION('',$,#11059);
#10999=PRODUCT_DEFINITION_FORMATION('',$,#11060);
#11000=PRODUCT_DEFINITION_FORMATION('',$,#11061);
#11001=PRODUCT_DEFINITION_FORMATION('',$,#11062);
#11002=PRODUCT_DEFINITION_FORMATION('',$,#11063);
#11003=PRODUCT_DEFINITION_FORMATION('',$,#11064);
#11004=PRODUCT_DEFINITION_FORMATION('',$,#11065);
#11005=PRODUCT_DEFINITION_FORMATION('',$,#11066);
#11006=PRODUCT_DEFINITION_FORMATION('',$,#11067);
#11007=PRODUCT_DEFINITION_FORMATION('',$,#11068);
#11008=PRODUCT_DEFINITION_FORMATION('',$,#11069);
#11009=PRODUCT_DEFINITION_FORMATION('',$,#11070);
#11010=PRODUCT_DEFINITION_FORMATION('',$,#11071);
#11011=PRODUCT_DEFINITION_FORMATION('',$,#11072);
#11012=PRODUCT_RELATED_PRODUCT_CATEGORY('PAT-025','PAT-025',(#11044));
#11013=PRODUCT_RELATED_PRODUCT_CATEGORY('Pillow block stand',
'Pillow block stand',(#11045));
#11014=PRODUCT_RELATED_PRODUCT_CATEGORY('Base channel','Base channel',(#11046));
#11015=PRODUCT_RELATED_PRODUCT_CATEGORY('Bonded pad','Bonded pad',(#11047));
#11016=PRODUCT_RELATED_PRODUCT_CATEGORY('Bonded pad (1)',
'Bonded pad (1)',(#11048));
#11017=PRODUCT_RELATED_PRODUCT_CATEGORY('Mounting bush','Mounting bush',
(#11049));
#11018=PRODUCT_RELATED_PRODUCT_CATEGORY('Mounting bush (1)',
'Mounting bush (1)',(#11050));
#11019=PRODUCT_RELATED_PRODUCT_CATEGORY('Mounting bush (2)',
'Mounting bush (2)',(#11051));
#11020=PRODUCT_RELATED_PRODUCT_CATEGORY('Mounting bush (3)',
'Mounting bush (3)',(#11052));
#11021=PRODUCT_RELATED_PRODUCT_CATEGORY(
'Pillow Block Bearing - 20 mm Bore','Pillow Block Bearing - 20 mm Bore',
(#11053));
#11022=PRODUCT_RELATED_PRODUCT_CATEGORY('Housing','Housing',(#11054));
#11023=PRODUCT_RELATED_PRODUCT_CATEGORY('Insert bearing',
'Insert bearing',(#11055));
#11024=PRODUCT_RELATED_PRODUCT_CATEGORY('Flat Washer - M8',
'Flat Washer - M8',(#11056));
#11025=PRODUCT_RELATED_PRODUCT_CATEGORY('M8x25 Bolt','M8x25 Bolt',(#11057));
#11026=PRODUCT_RELATED_PRODUCT_CATEGORY('Countershaft rotor',
'Countershaft rotor',(#11058));
#11027=PRODUCT_RELATED_PRODUCT_CATEGORY('Stepped countershaft',
'Stepped countershaft',(#11059));
#11028=PRODUCT_RELATED_PRODUCT_CATEGORY('Left spacer','Left spacer',(#11060));
#11029=PRODUCT_RELATED_PRODUCT_CATEGORY('Right spacer','Right spacer',(#11061));
#11030=PRODUCT_RELATED_PRODUCT_CATEGORY('Left end shim','Left end shim',
(#11062));
#11031=PRODUCT_RELATED_PRODUCT_CATEGORY('End keeper','End keeper',(#11063));
#11032=PRODUCT_RELATED_PRODUCT_CATEGORY('End keeper (1)',
'End keeper (1)',(#11064));
#11033=PRODUCT_RELATED_PRODUCT_CATEGORY('Keyed drive hub',
'Keyed drive hub',(#11065));
#11034=PRODUCT_RELATED_PRODUCT_CATEGORY('Bearing collar',
'Bearing collar',(#11066));
#11035=PRODUCT_RELATED_PRODUCT_CATEGORY('Bearing collar (1)',
'Bearing collar (1)',(#11067));
#11036=PRODUCT_RELATED_PRODUCT_CATEGORY(
'Timing Pulley - 2 mm Pitch, 40 Teeth, 12 mm Bore',
'Timing Pulley - 2 mm Pitch, 40 Teeth, 12 mm Bore',(#11068));
#11037=PRODUCT_RELATED_PRODUCT_CATEGORY('Key 4x4x14','Key 4x4x14',(#11069));
#11038=PRODUCT_RELATED_PRODUCT_CATEGORY('Cap Screw - M5x20',
'Cap Screw - M5x20',(#11070));
#11039=PRODUCT_RELATED_PRODUCT_CATEGORY('Key 6x6x20','Key 6x6x20',(#11071));
#11040=PRODUCT_RELATED_PRODUCT_CATEGORY('Socket Set Screw - M5x8',
'Socket Set Screw - M5x8',(#11072));
#11041=APPLICATION_PROTOCOL_DEFINITION('international standard',
'automotive_design',2009,#11042);
#11042=APPLICATION_CONTEXT(
'Core Data for Automotive Mechanical Design Process');
#11043=PRODUCT_CONTEXT('part definition',#11042,'mechanical');
#11044=PRODUCT('PAT-025',
'PAT-025','PAT-025',(#11043));
#11045=PRODUCT('Pillow block stand','Pillow block stand',
'Pillow block stand',(#11043));
#11046=PRODUCT('Base channel','Base channel','Base channel',(#11043));
#11047=PRODUCT('Bonded pad','Bonded pad','Bonded pad',(#11043));
#11048=PRODUCT('Bonded pad (1)','Bonded pad (1)','Bonded pad (1)',(#11043));
#11049=PRODUCT('Mounting bush','Mounting bush','Mounting bush',(#11043));
#11050=PRODUCT('Mounting bush (1)','Mounting bush (1)','Mounting bush (1)',(#11043));
#11051=PRODUCT('Mounting bush (2)','Mounting bush (2)','Mounting bush (2)',(#11043));
#11052=PRODUCT('Mounting bush (3)','Mounting bush (3)','Mounting bush (3)',(#11043));
#11053=PRODUCT('Pillow Block Bearing - 20 mm Bore',
'Pillow Block Bearing - 20 mm Bore','Pillow Block Bearing - 20 mm Bore',
(#11043));
#11054=PRODUCT('Housing','Housing','Housing',(#11043));
#11055=PRODUCT('Insert bearing','Insert bearing','Insert bearing',(#11043));
#11056=PRODUCT('Flat Washer - M8','Flat Washer - M8','Flat Washer - M8',
(#11043));
#11057=PRODUCT('M8x25 Bolt','M8x25 Bolt','M8x25 Bolt',(#11043));
#11058=PRODUCT('Countershaft rotor','Countershaft rotor',
'Countershaft rotor',(#11043));
#11059=PRODUCT('Stepped countershaft','Stepped countershaft',
'Stepped countershaft',(#11043));
#11060=PRODUCT('Left spacer','Left spacer','Left spacer',(#11043));
#11061=PRODUCT('Right spacer','Right spacer','Right spacer',(#11043));
#11062=PRODUCT('Left end shim','Left end shim','Left end shim',(#11043));
#11063=PRODUCT('End keeper','End keeper','End keeper',(#11043));
#11064=PRODUCT('End keeper (1)','End keeper (1)','End keeper (1)',(#11043));
#11065=PRODUCT('Keyed drive hub','Keyed drive hub','Keyed drive hub',(#11043));
#11066=PRODUCT('Bearing collar','Bearing collar','Bearing collar',(#11043));
#11067=PRODUCT('Bearing collar (1)','Bearing collar (1)','Bearing collar (1)',
(#11043));
#11068=PRODUCT('Timing Pulley - 2 mm Pitch, 40 Teeth, 12 mm Bore',
'Timing Pulley - 2 mm Pitch, 40 Teeth, 12 mm Bore',
'Timing Pulley - 2 mm Pitch, 40 Teeth, 12 mm Bore',(#11043));
#11069=PRODUCT('Key 4x4x14','Key 4x4x14','Key 4x4x14',(#11043));
#11070=PRODUCT('Cap Screw - M5x20','Cap Screw - M5x20',
'Cap Screw - M5x20',(#11043));
#11071=PRODUCT('Key 6x6x20','Key 6x6x20','Key 6x6x20',(#11043));
#11072=PRODUCT('Socket Set Screw - M5x8','Socket Set Screw - M5x8',
'Socket Set Screw - M5x8',(#11043));
#11073=PRESENTATION_STYLE_ASSIGNMENT((#11078));
#11074=PRESENTATION_STYLE_ASSIGNMENT((#11079));
#11075=PRESENTATION_STYLE_ASSIGNMENT((#11080));
#11076=PRESENTATION_STYLE_ASSIGNMENT((#11081));
#11077=PRESENTATION_STYLE_ASSIGNMENT((#11082));
#11078=SURFACE_STYLE_USAGE(.BOTH.,#11083);
#11079=SURFACE_STYLE_USAGE(.BOTH.,#11084);
#11080=SURFACE_STYLE_USAGE(.BOTH.,#11085);
#11081=SURFACE_STYLE_USAGE(.BOTH.,#11086);
#11082=SURFACE_STYLE_USAGE(.BOTH.,#11087);
#11083=SURFACE_SIDE_STYLE('',(#11088));
#11084=SURFACE_SIDE_STYLE('',(#11089));
#11085=SURFACE_SIDE_STYLE('',(#11090));
#11086=SURFACE_SIDE_STYLE('',(#11091));
#11087=SURFACE_SIDE_STYLE('',(#11092));
#11088=SURFACE_STYLE_FILL_AREA(#11093);
#11089=SURFACE_STYLE_FILL_AREA(#11094);
#11090=SURFACE_STYLE_FILL_AREA(#11095);
#11091=SURFACE_STYLE_FILL_AREA(#11096);
#11092=SURFACE_STYLE_FILL_AREA(#11097);
#11093=FILL_AREA_STYLE('Steel - Satin',(#11098));
#11094=FILL_AREA_STYLE('CAD Library Painted - Deep blue',(#11099));
#11095=FILL_AREA_STYLE('CAD Library Painted - Graphite',(#11100));
#11096=FILL_AREA_STYLE('CAD Library Painted - Engineering blue',(#11101));
#11097=FILL_AREA_STYLE('CAD Library Painted - Steel gray',(#11102));
#11098=FILL_AREA_STYLE_COLOUR('Steel - Satin',#11103);
#11099=FILL_AREA_STYLE_COLOUR('CAD Library Painted - Deep blue',#11104);
#11100=FILL_AREA_STYLE_COLOUR('CAD Library Painted - Graphite',#11105);
#11101=FILL_AREA_STYLE_COLOUR('CAD Library Painted - Engineering blue',
#11106);
#11102=FILL_AREA_STYLE_COLOUR('CAD Library Painted - Steel gray',#11107);
#11103=COLOUR_RGB('Steel - Satin',0.627450980392157,0.627450980392157,0.627450980392157);
#11104=COLOUR_RGB('CAD Library Painted - Deep blue',0.0784313725490196,
0.203921568627451,0.349019607843137);
#11105=COLOUR_RGB('CAD Library Painted - Graphite',0.168627450980392,0.192156862745098,
0.231372549019608);
#11106=COLOUR_RGB('CAD Library Painted - Engineering blue',0.12156862745098,
0.356862745098039,0.6);
#11107=COLOUR_RGB('CAD Library Painted - Steel gray',0.592156862745098,
0.631372549019608,0.67843137254902);
#11108=COLOUR_RGB('Dark Blue',0.08,0.2,0.34);
#11109=FILL_AREA_STYLE_COLOUR('',#11108);
#11110=FILL_AREA_STYLE('',(#11109));
#11111=SURFACE_STYLE_FILL_AREA(#11110);
#11112=SURFACE_SIDE_STYLE('',(#11111));
#11113=SURFACE_STYLE_USAGE(.BOTH.,#11112);
#11114=PRESENTATION_STYLE_ASSIGNMENT((#11113));
#11115=COLOUR_RGB('Light Blue',0.38,0.62,0.78);
#11116=FILL_AREA_STYLE_COLOUR('',#11115);
#11117=FILL_AREA_STYLE('',(#11116));
#11118=SURFACE_STYLE_FILL_AREA(#11117);
#11119=SURFACE_SIDE_STYLE('',(#11118));
#11120=SURFACE_STYLE_USAGE(.BOTH.,#11119);
#11121=PRESENTATION_STYLE_ASSIGNMENT((#11120));
#11122=COLOUR_RGB('Sky Blue',0.24,0.69,0.87);
#11123=FILL_AREA_STYLE_COLOUR('',#11122);
#11124=FILL_AREA_STYLE('',(#11123));
#11125=SURFACE_STYLE_FILL_AREA(#11124);
#11126=SURFACE_SIDE_STYLE('',(#11125));
#11127=SURFACE_STYLE_USAGE(.BOTH.,#11126);
#11128=PRESENTATION_STYLE_ASSIGNMENT((#11127));
#11129=COLOUR_RGB('Grey',0.48,0.52,0.57);
#11130=FILL_AREA_STYLE_COLOUR('',#11129);
#11131=FILL_AREA_STYLE('',(#11130));
#11132=SURFACE_STYLE_FILL_AREA(#11131);
#11133=SURFACE_SIDE_STYLE('',(#11132));
#11134=SURFACE_STYLE_USAGE(.BOTH.,#11133);
#11135=PRESENTATION_STYLE_ASSIGNMENT((#11134));
#11136=COLOUR_RGB('Black',0.12,0.14,0.17);
#11137=FILL_AREA_STYLE_COLOUR('',#11136);
#11138=FILL_AREA_STYLE('',(#11137));
#11139=SURFACE_STYLE_FILL_AREA(#11138);
#11140=SURFACE_SIDE_STYLE('',(#11139));
#11141=SURFACE_STYLE_USAGE(.BOTH.,#11140);
#11142=PRESENTATION_STYLE_ASSIGNMENT((#11141));
#11143=COLOUR_RGB('Off White',0.89,0.88,0.83);
#11144=FILL_AREA_STYLE_COLOUR('',#11143);
#11145=FILL_AREA_STYLE('',(#11144));
#11146=SURFACE_STYLE_FILL_AREA(#11145);
#11147=SURFACE_SIDE_STYLE('',(#11146));
#11148=SURFACE_STYLE_USAGE(.BOTH.,#11147);
#11149=PRESENTATION_STYLE_ASSIGNMENT((#11148));
ENDSEC;
END-ISO-10303-21;
